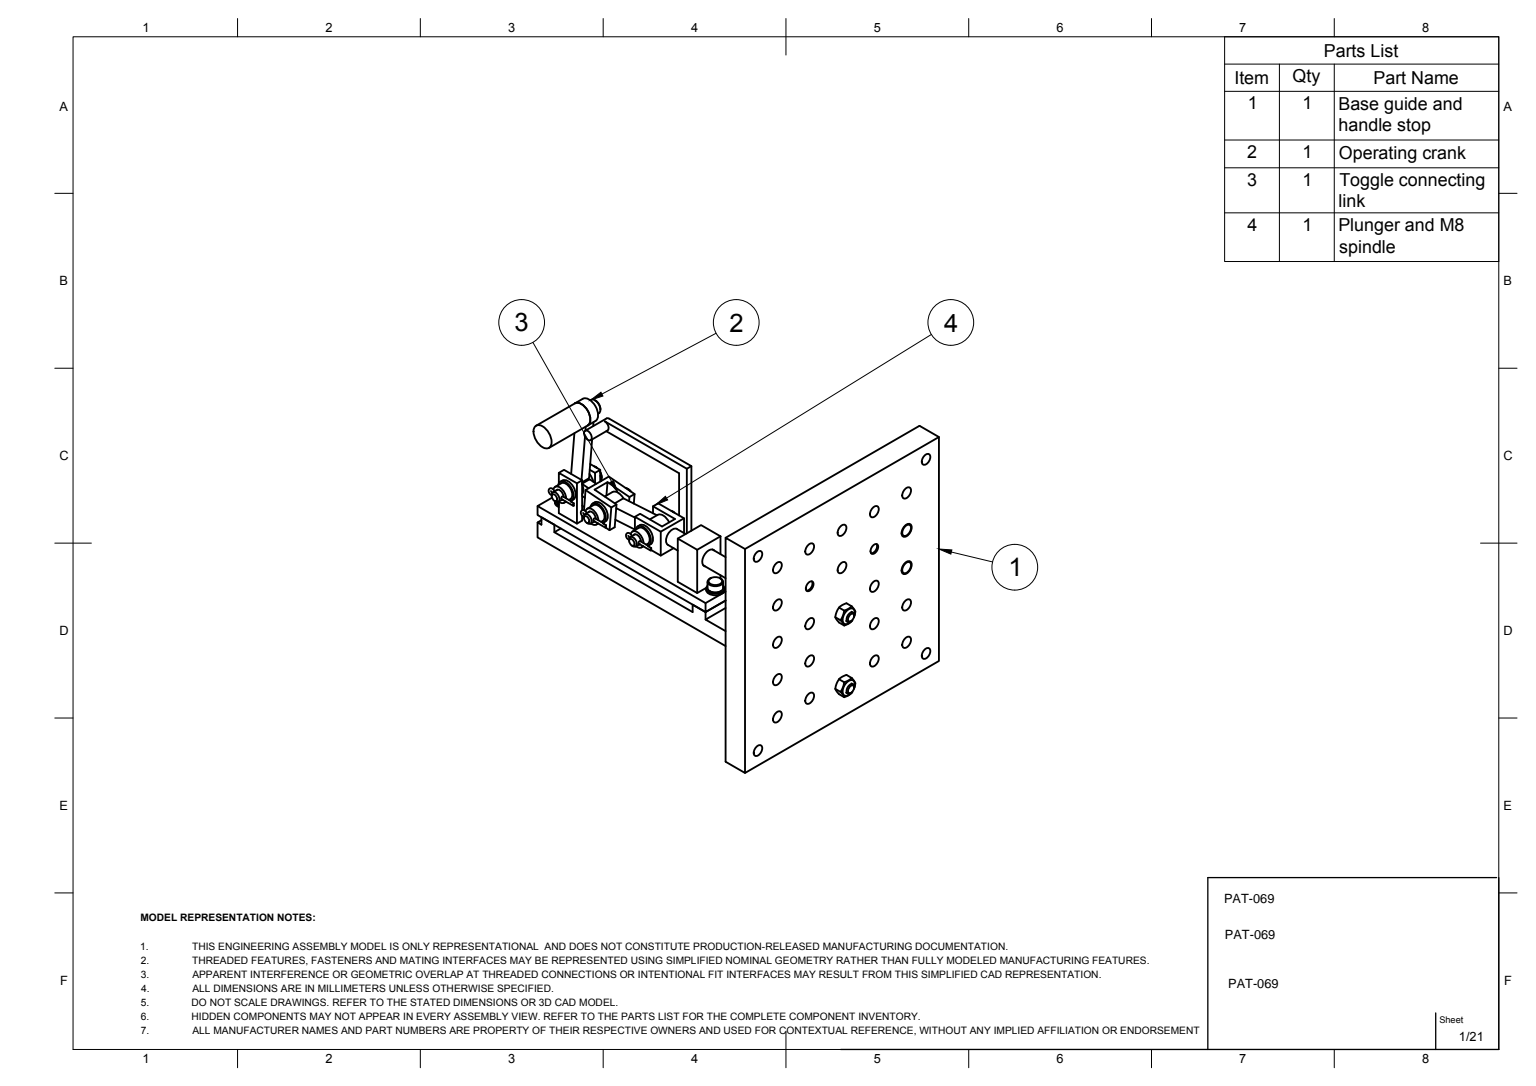
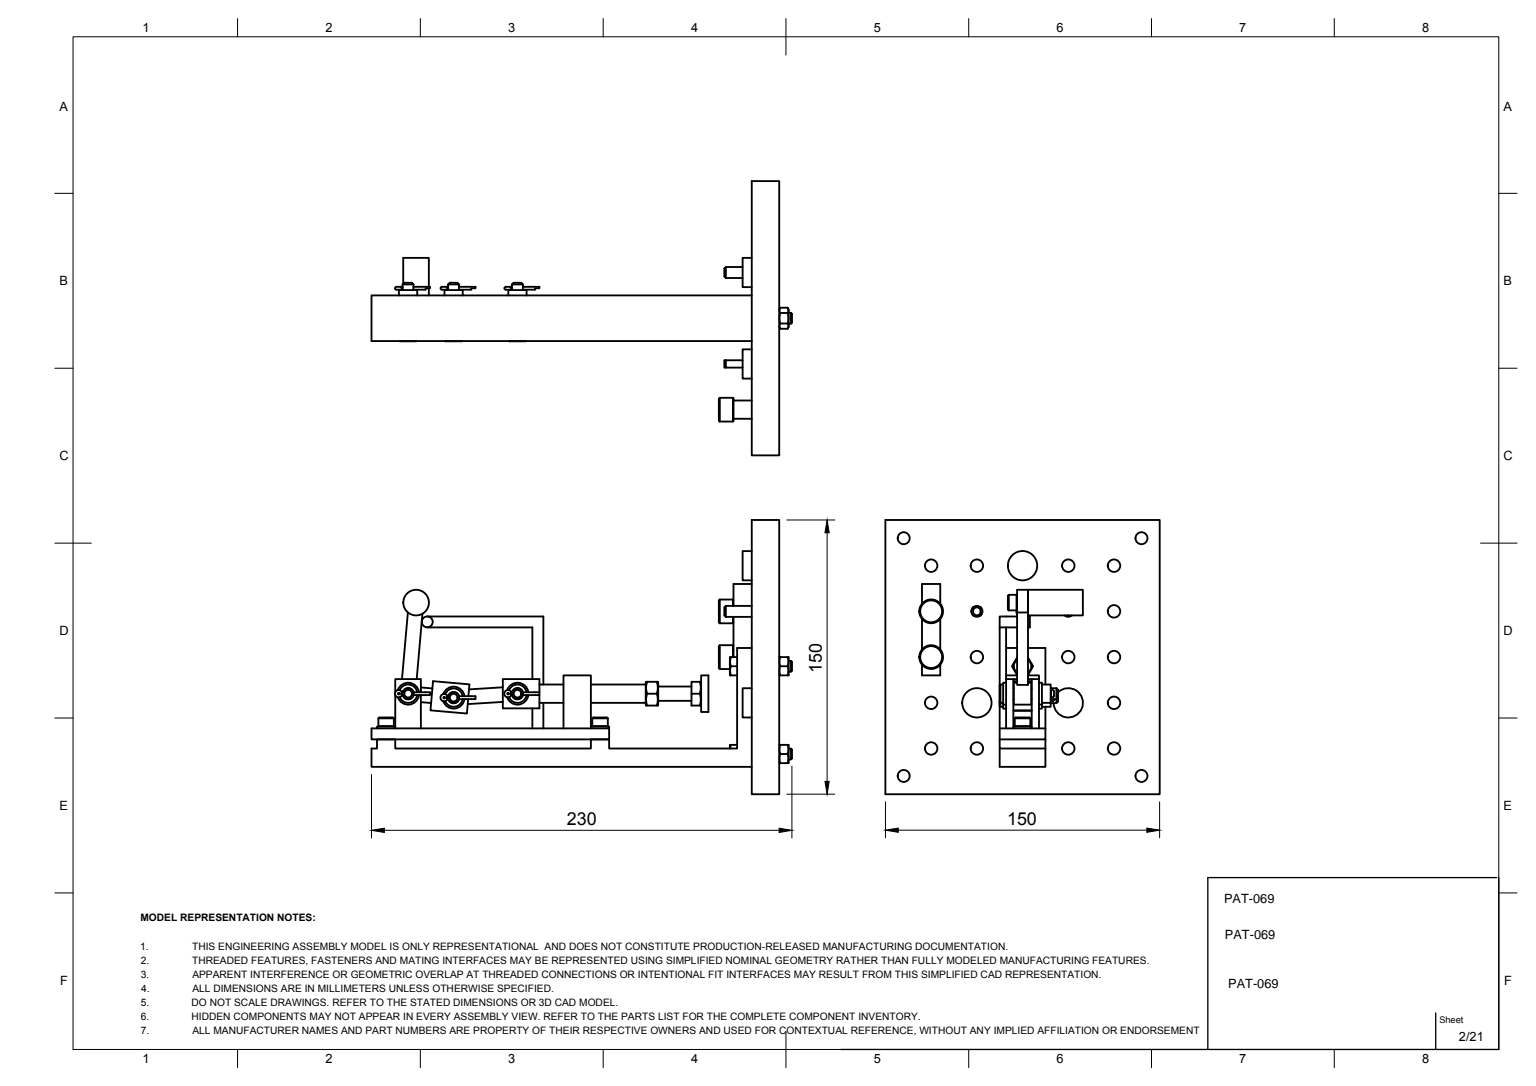
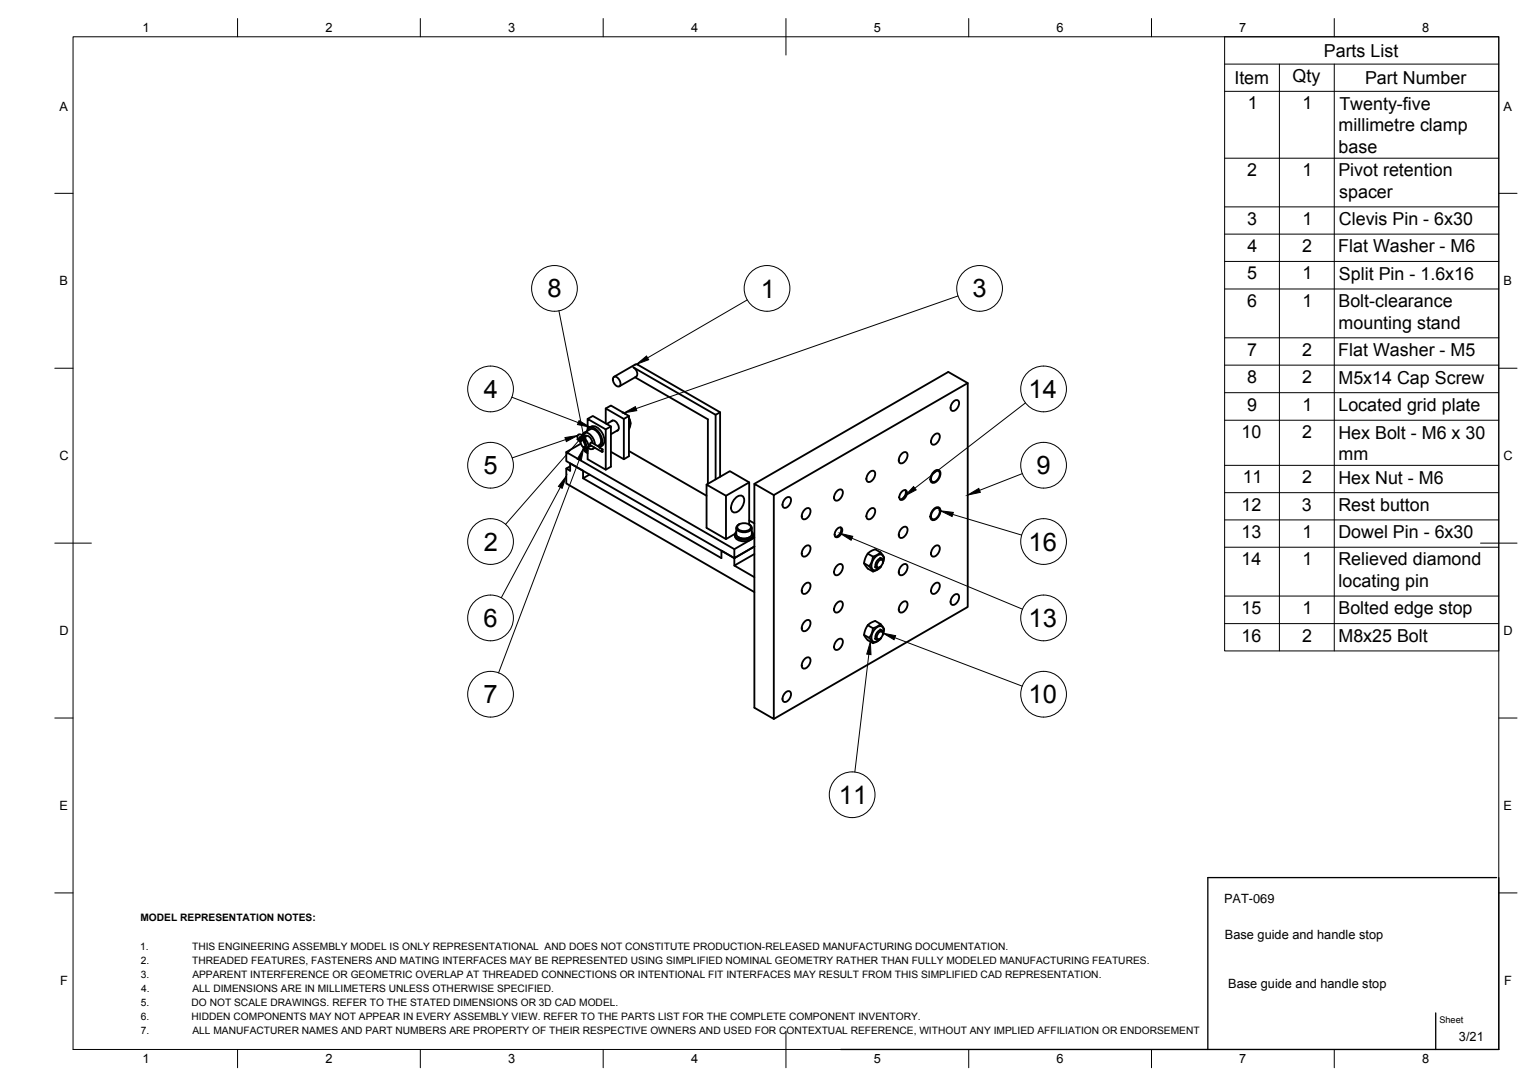
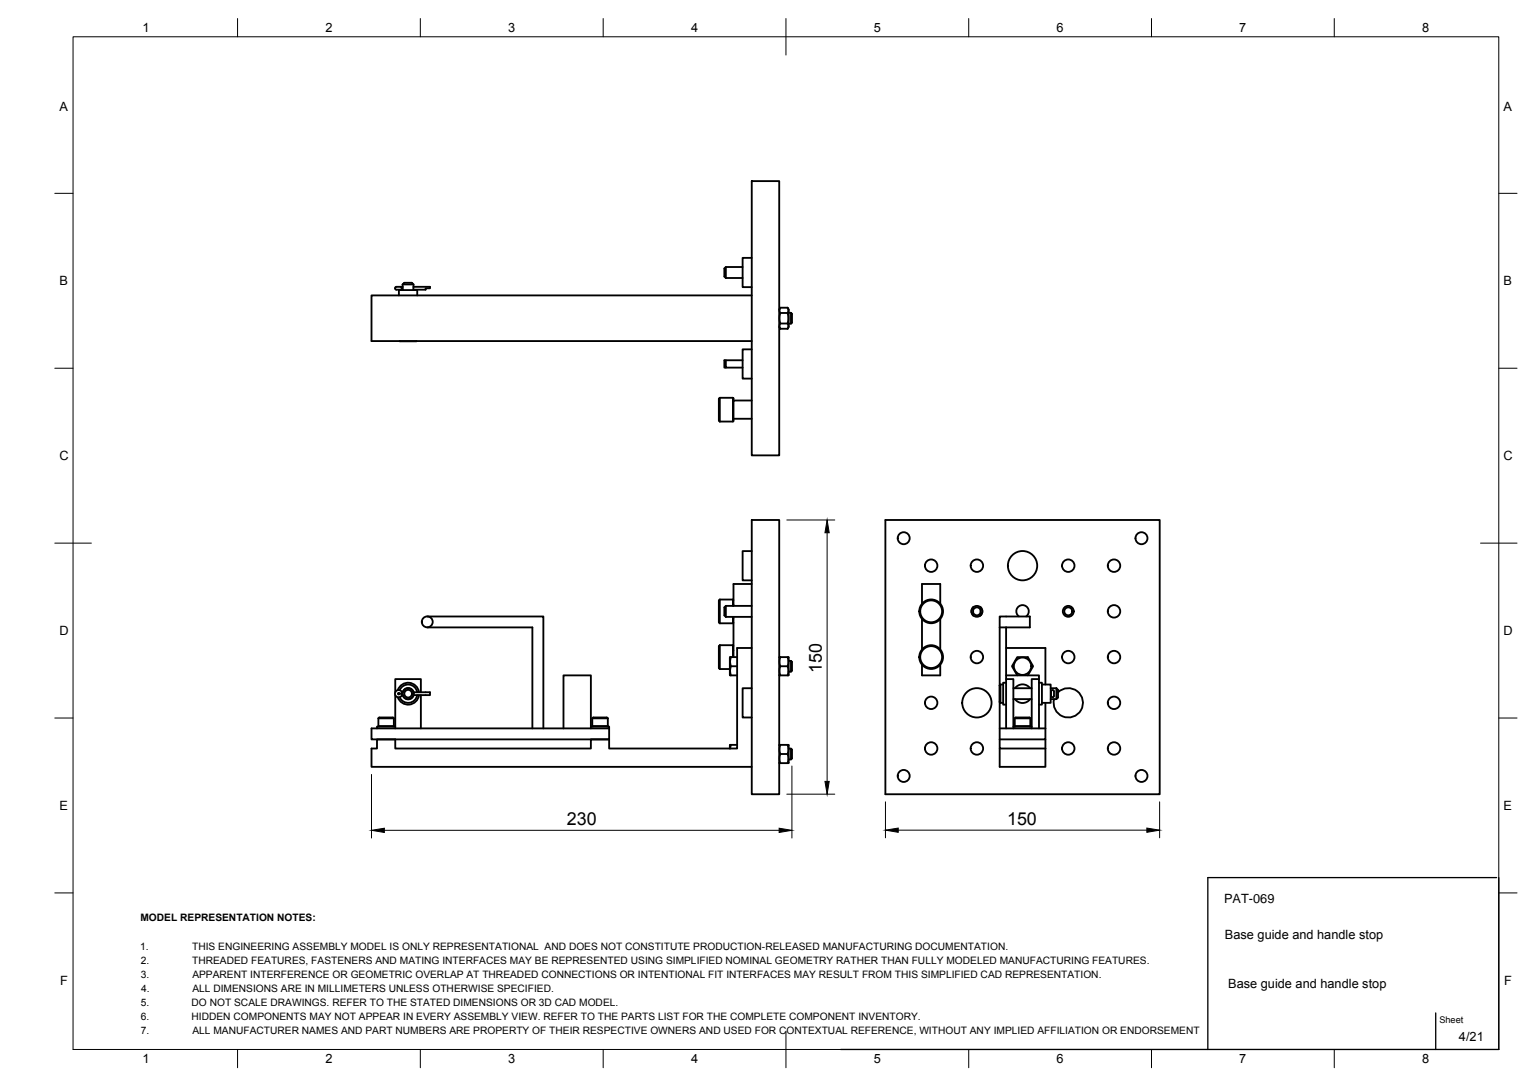
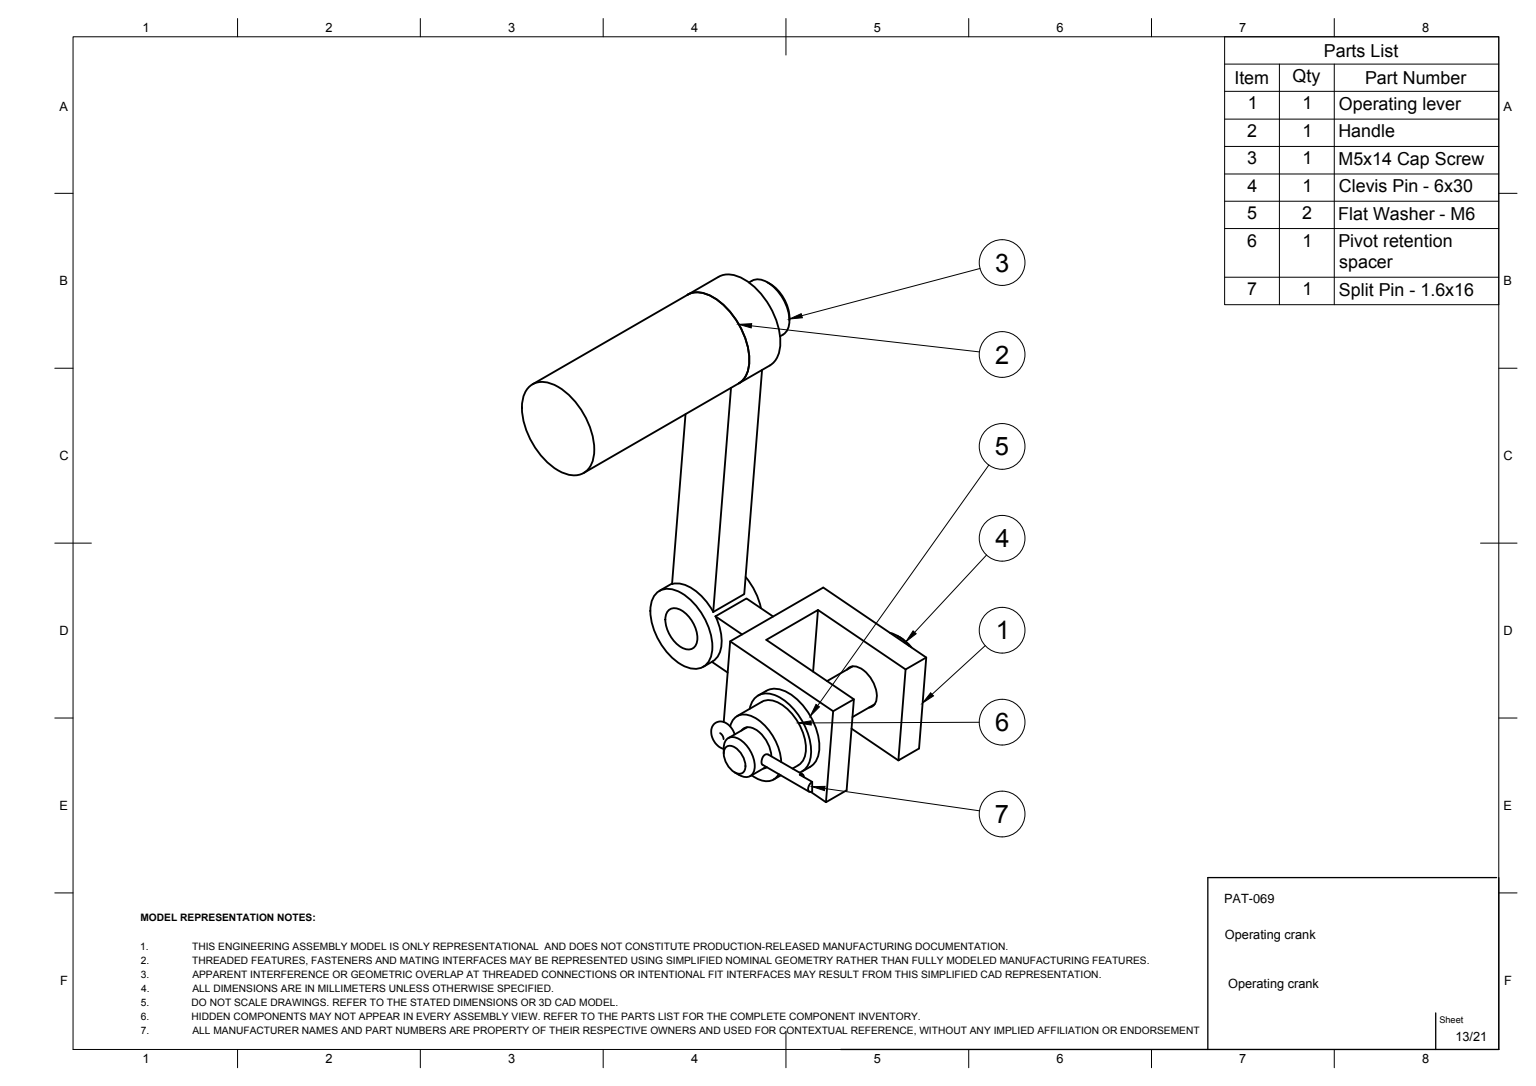
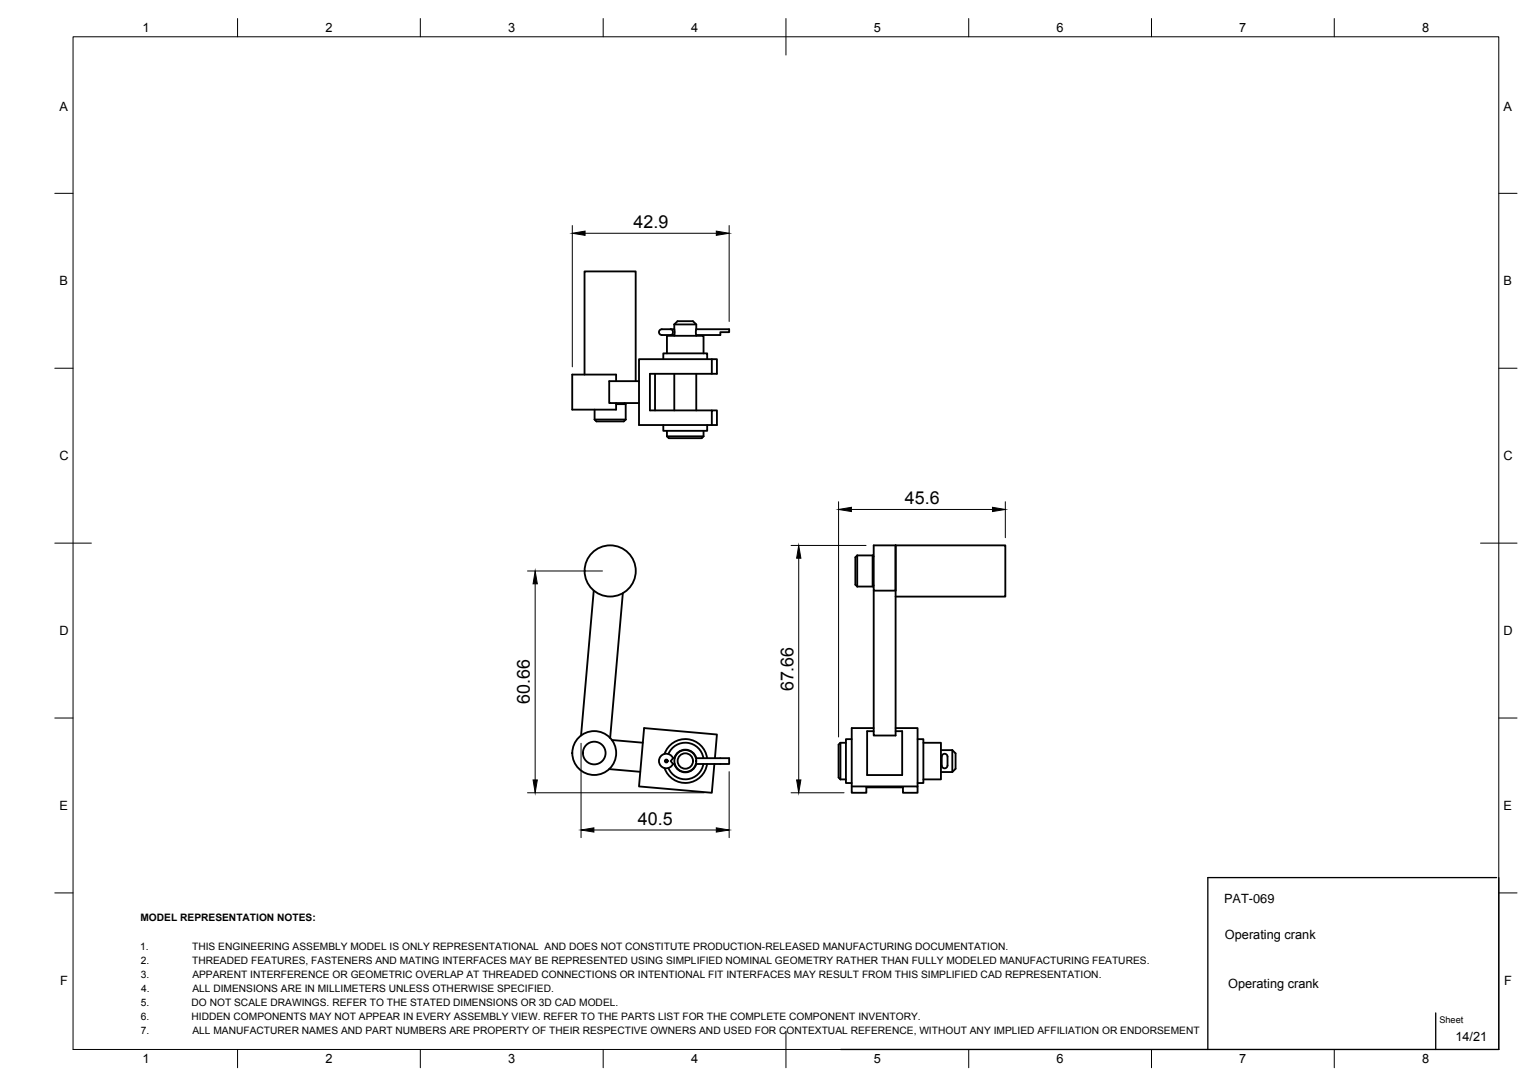
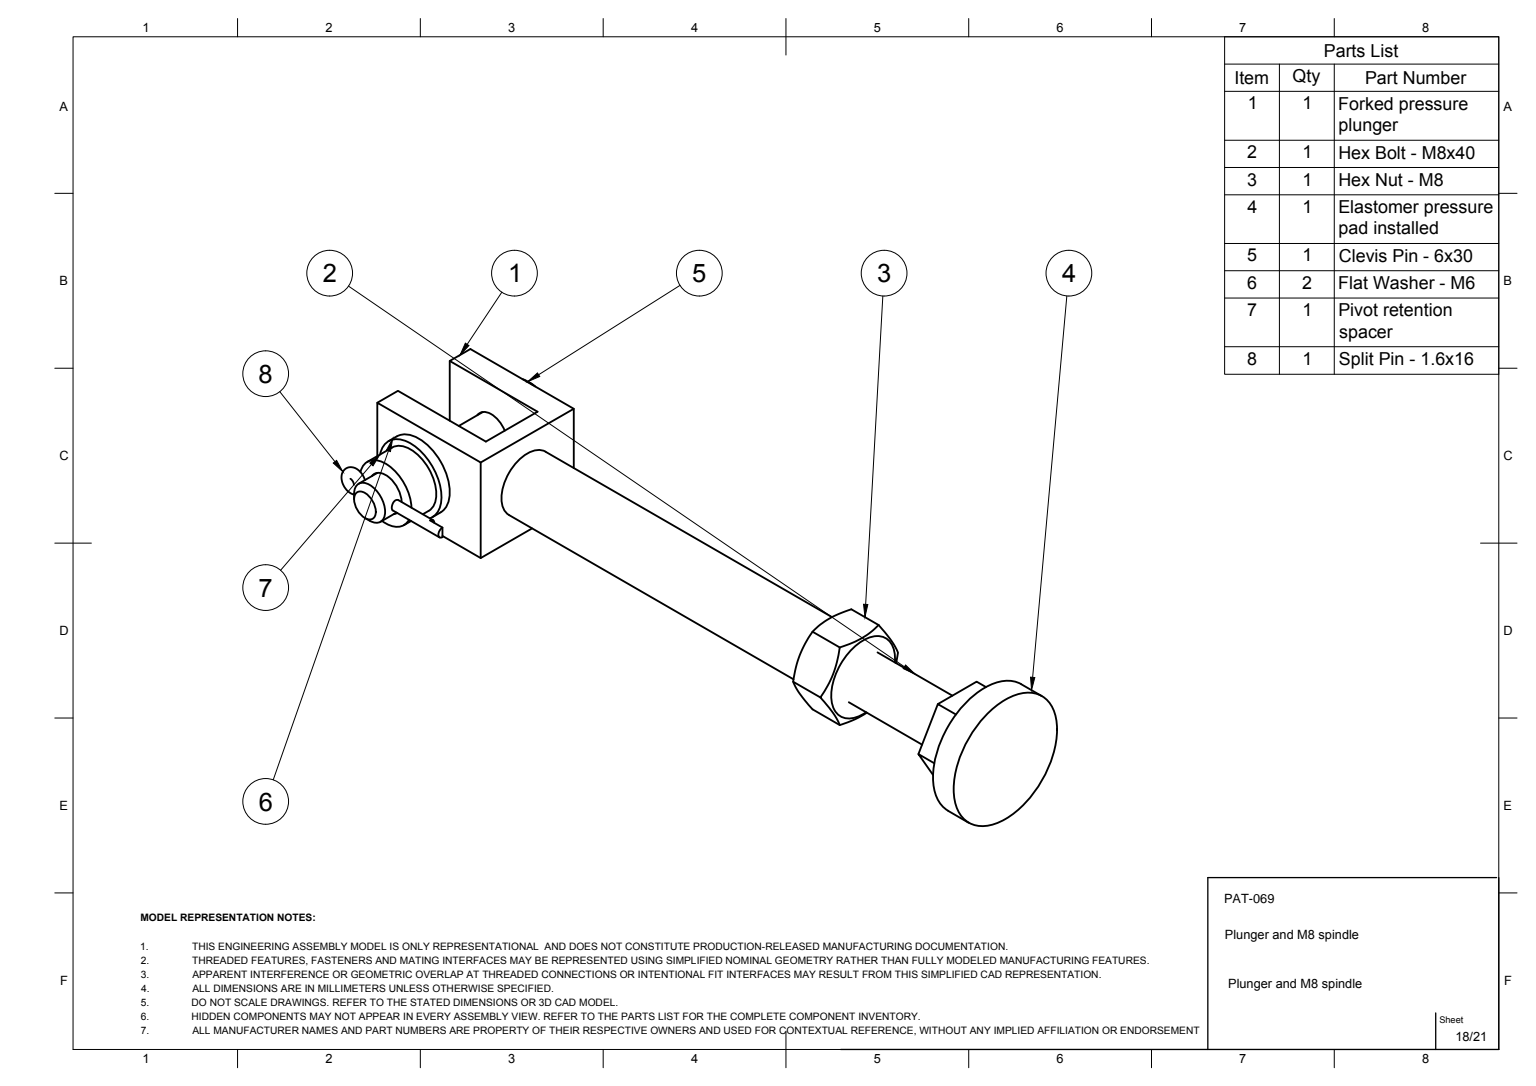
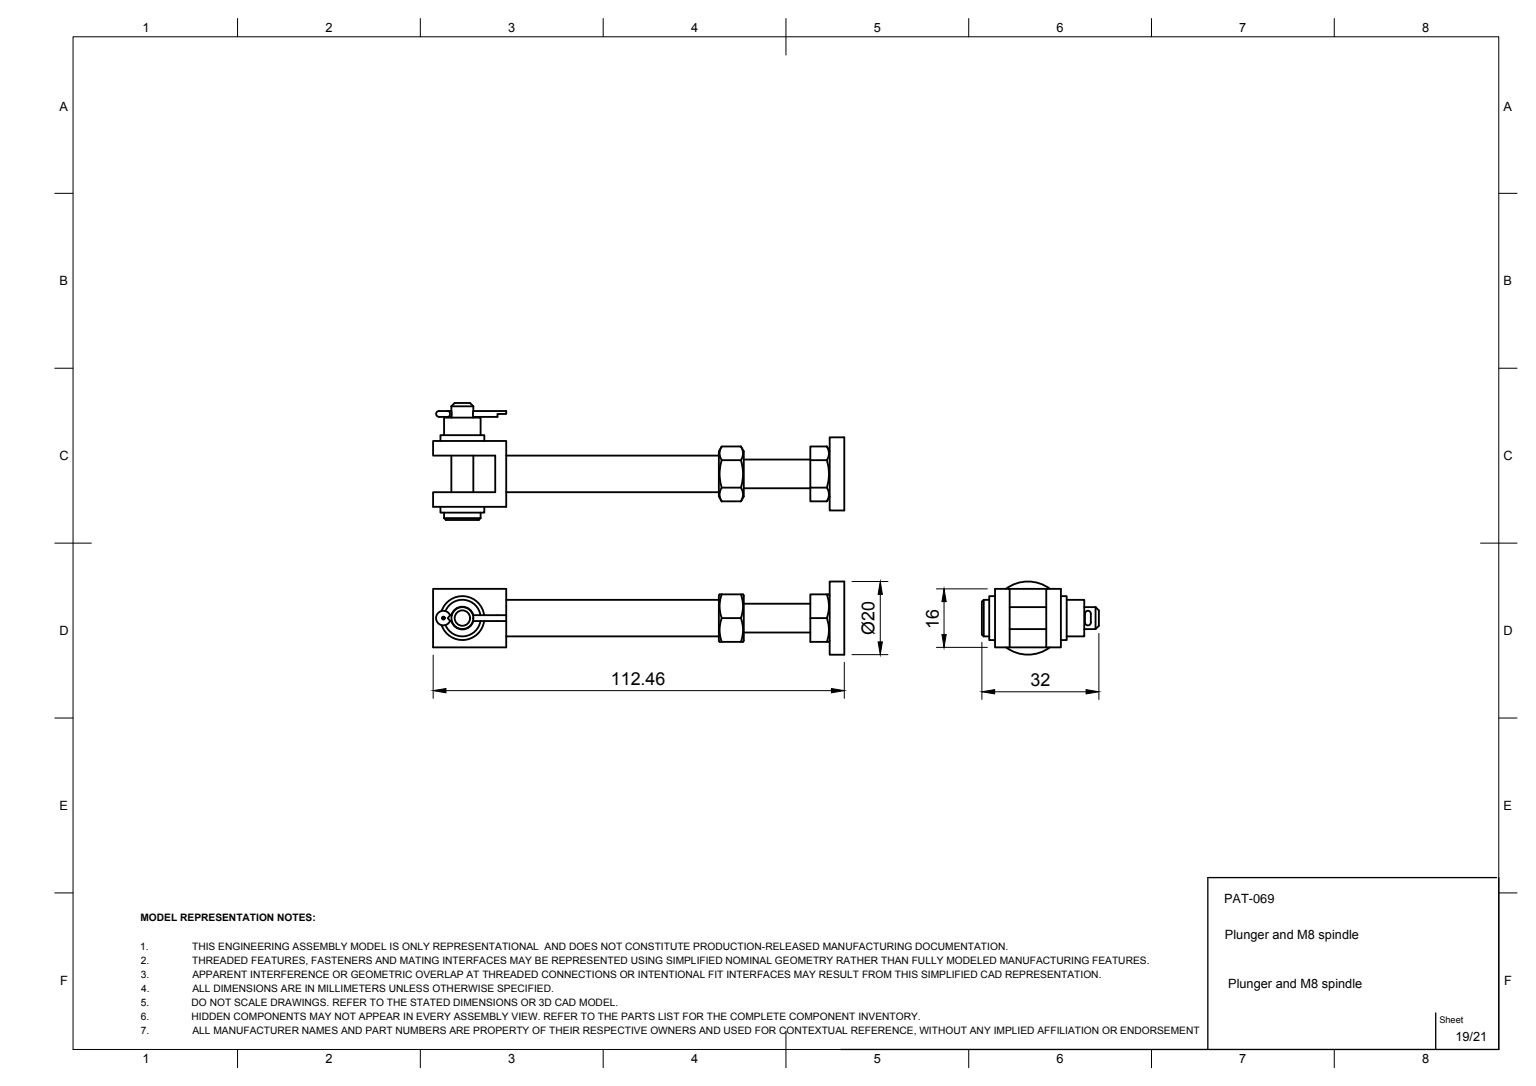
ISO-10303-21;
HEADER;
/* Generated by software containing ST-Developer
 * from STEP Tools, Inc. (www.steptools.com) 
 */

FILE_DESCRIPTION(
/* description */ ('Located fixture plate with toggle clamp'),
/* implementation_level */ '2;1');

FILE_NAME(
/* name */ 'PAT-069',
/* time_stamp */ '2026-10-27T21:36:12-07:00',
/* author */ (''),
/* organization */ (''),
/* preprocessor_version */ 'ST-DEVELOPER v20.2',
/* originating_system */ 'Autodesk Translation Framework v15.17.0.0',
/* authorisation */ '');

FILE_SCHEMA (('AUTOMOTIVE_DESIGN { 1 0 10303 214 3 1 1 }'));
ENDSEC;

DATA;
#10=MECHANICAL_DESIGN_GEOMETRIC_PRESENTATION_REPRESENTATION('',(#321,#322,
#323,#324,#325,#326,#327,#328,#329,#330,#331,#332,#333,#334,#335,#336,#337,
#338,#339,#340,#341,#342,#343,#344),#9285);
#11=TOROIDAL_SURFACE('',#5974,0.12,0.08);
#12=B_SPLINE_CURVE_WITH_KNOTS('',3,(#8976,#8977,#8978,#8979,#8980,#8981,
#8982,#8983,#8984,#8985),.UNSPECIFIED.,.F.,.F.,(4,2,2,2,4),(0.,0.0302963256060356,
0.0605926512120712,0.090883446720838,0.121174242229605),.UNSPECIFIED.);
#13=B_SPLINE_CURVE_WITH_KNOTS('',3,(#8988,#8989,#8990,#8991,#8992,#8993,
#8994,#8995,#8996,#8997,#8998,#8999,#9000,#9001,#9002,#9003,#9004,#9005,
#9006,#9007,#9008,#9009,#9010,#9011,#9012,#9013,#9014,#9015,#9016,#9017,
#9018,#9019,#9020,#9021),.UNSPECIFIED.,.T.,.F.,(4,2,2,2,2,2,2,2,2,2,2,2,
2,2,2,2,4),(0.,0.0302963256060358,0.0605926512120716,0.0908834467208383,
0.121174242229605,0.151465037738372,0.181755833247138,0.212052158853174,
0.24234848445921,0.272644810065246,0.302941135671282,0.333231931180048,
0.363522726688815,0.393813522197582,0.424104317706349,0.454400643312384,
0.48469696891842),.UNSPECIFIED.);
#14=B_SPLINE_CURVE_WITH_KNOTS('',3,(#9023,#9024,#9025,#9026,#9027,#9028,
#9029,#9030,#9031,#9032),.UNSPECIFIED.,.F.,.F.,(4,2,2,2,4),(0.363522726688815,
0.393813522197581,0.424104317706348,0.454400643312384,0.48469696891842),
 .UNSPECIFIED.);
#15=B_SPLINE_CURVE_WITH_KNOTS('',3,(#9033,#9034,#9035,#9036,#9037,#9038,
#9039,#9040,#9041,#9042,#9043,#9044,#9045,#9046,#9047,#9048,#9049,#9050),
 .UNSPECIFIED.,.F.,.F.,(4,2,2,2,2,2,2,2,4),(0.121174242229605,0.151465037738371,
0.181755833247138,0.212052158853174,0.24234848445921,0.272644810065246,
0.302941135671281,0.333231931180048,0.363522726688815),.UNSPECIFIED.);
#16=B_SPLINE_CURVE_WITH_KNOTS('',3,(#9112,#9113,#9114,#9115,#9116,#9117,
#9118,#9119,#9120,#9121,#9122,#9123,#9124,#9125,#9126,#9127,#9128,#9129,
#9130,#9131,#9132,#9133,#9134,#9135,#9136,#9137),.UNSPECIFIED.,.F.,.F.,
(4,2,2,2,2,2,2,2,2,2,2,2,4),(-0.00054581412719389,0.,0.0281583564005144,
0.0618496465371181,0.0905865724114538,0.120694112793616,0.144966158459363,
0.16923820412511,0.199345744507272,0.228082670381608,0.261773960518212,
0.289932316918681,0.290478131045882),.UNSPECIFIED.);
#17=B_SPLINE_CURVE_WITH_KNOTS('',3,(#9138,#9139,#9140,#9141,#9142,#9143,
#9144,#9145,#9146,#9147,#9148,#9149,#9150,#9151,#9152,#9153,#9154,#9155,
#9156,#9157,#9158,#9159,#9160,#9161,#9162,#9163),.UNSPECIFIED.,.F.,.F.,
(4,2,2,2,2,2,2,2,2,2,2,2,4),(-0.000545814127196571,0.,0.0281583564006391,
0.0618496465374156,0.0905865724118984,0.120694112794215,0.144966158460086,
0.169238204125958,0.199345744508275,0.228082670382758,0.261773960519534,
0.289932316920171,0.29047813104737),.UNSPECIFIED.);
#18=ITEM_DEFINED_TRANSFORMATION($,$,#5857,#5874);
#19=ITEM_DEFINED_TRANSFORMATION($,$,#5463,#5984);
#20=ITEM_DEFINED_TRANSFORMATION($,$,#5964,#5985);
#21=ITEM_DEFINED_TRANSFORMATION($,$,#5940,#5986);
#22=ITEM_DEFINED_TRANSFORMATION($,$,#5955,#5987);
#23=ITEM_DEFINED_TRANSFORMATION($,$,#5955,#5988);
#24=ITEM_DEFINED_TRANSFORMATION($,$,#5973,#5989);
#25=ITEM_DEFINED_TRANSFORMATION($,$,#5511,#5990);
#26=ITEM_DEFINED_TRANSFORMATION($,$,#5546,#5991);
#27=ITEM_DEFINED_TRANSFORMATION($,$,#5557,#5992);
#28=ITEM_DEFINED_TRANSFORMATION($,$,#5546,#5993);
#29=ITEM_DEFINED_TRANSFORMATION($,$,#5557,#5994);
#30=ITEM_DEFINED_TRANSFORMATION($,$,#5581,#5995);
#31=ITEM_DEFINED_TRANSFORMATION($,$,#5718,#5996);
#32=ITEM_DEFINED_TRANSFORMATION($,$,#5672,#5997);
#33=ITEM_DEFINED_TRANSFORMATION($,$,#5685,#5998);
#34=ITEM_DEFINED_TRANSFORMATION($,$,#5702,#5999);
#35=ITEM_DEFINED_TRANSFORMATION($,$,#5685,#6000);
#36=ITEM_DEFINED_TRANSFORMATION($,$,#5702,#6001);
#37=ITEM_DEFINED_TRANSFORMATION($,$,#5718,#6002);
#38=ITEM_DEFINED_TRANSFORMATION($,$,#5718,#6003);
#39=ITEM_DEFINED_TRANSFORMATION($,$,#5728,#6004);
#40=ITEM_DEFINED_TRANSFORMATION($,$,#5736,#6005);
#41=ITEM_DEFINED_TRANSFORMATION($,$,#5754,#6006);
#42=ITEM_DEFINED_TRANSFORMATION($,$,#5754,#6007);
#43=ITEM_DEFINED_TRANSFORMATION($,$,#5779,#6008);
#44=ITEM_DEFINED_TRANSFORMATION($,$,#5822,#6009);
#45=ITEM_DEFINED_TRANSFORMATION($,$,#5832,#6010);
#46=ITEM_DEFINED_TRANSFORMATION($,$,#5940,#6011);
#47=ITEM_DEFINED_TRANSFORMATION($,$,#5955,#6012);
#48=ITEM_DEFINED_TRANSFORMATION($,$,#5955,#6013);
#49=ITEM_DEFINED_TRANSFORMATION($,$,#5964,#6014);
#50=ITEM_DEFINED_TRANSFORMATION($,$,#5973,#6015);
#51=ITEM_DEFINED_TRANSFORMATION($,$,#5876,#6016);
#52=ITEM_DEFINED_TRANSFORMATION($,$,#5901,#6017);
#53=ITEM_DEFINED_TRANSFORMATION($,$,#5918,#6018);
#54=ITEM_DEFINED_TRANSFORMATION($,$,#5934,#6019);
#55=ITEM_DEFINED_TRANSFORMATION($,$,#5940,#6020);
#56=ITEM_DEFINED_TRANSFORMATION($,$,#5955,#6021);
#57=ITEM_DEFINED_TRANSFORMATION($,$,#5955,#6022);
#58=ITEM_DEFINED_TRANSFORMATION($,$,#5964,#6023);
#59=ITEM_DEFINED_TRANSFORMATION($,$,#5973,#6024);
#60=ITEM_DEFINED_TRANSFORMATION($,$,#5462,#6025);
#61=ITEM_DEFINED_TRANSFORMATION($,$,#5778,#6026);
#62=ITEM_DEFINED_TRANSFORMATION($,$,#5856,#6027);
#63=ITEM_DEFINED_TRANSFORMATION($,$,#5875,#6028);
#64=(
REPRESENTATION_RELATIONSHIP($,$,#9413,#9412)
REPRESENTATION_RELATIONSHIP_WITH_TRANSFORMATION(#18)
SHAPE_REPRESENTATION_RELATIONSHIP()
);
#65=(
REPRESENTATION_RELATIONSHIP($,$,#9396,#9395)
REPRESENTATION_RELATIONSHIP_WITH_TRANSFORMATION(#19)
SHAPE_REPRESENTATION_RELATIONSHIP()
);
#66=(
REPRESENTATION_RELATIONSHIP($,$,#9421,#9395)
REPRESENTATION_RELATIONSHIP_WITH_TRANSFORMATION(#20)
SHAPE_REPRESENTATION_RELATIONSHIP()
);
#67=(
REPRESENTATION_RELATIONSHIP($,$,#9419,#9395)
REPRESENTATION_RELATIONSHIP_WITH_TRANSFORMATION(#21)
SHAPE_REPRESENTATION_RELATIONSHIP()
);
#68=(
REPRESENTATION_RELATIONSHIP($,$,#9420,#9395)
REPRESENTATION_RELATIONSHIP_WITH_TRANSFORMATION(#22)
SHAPE_REPRESENTATION_RELATIONSHIP()
);
#69=(
REPRESENTATION_RELATIONSHIP($,$,#9420,#9395)
REPRESENTATION_RELATIONSHIP_WITH_TRANSFORMATION(#23)
SHAPE_REPRESENTATION_RELATIONSHIP()
);
#70=(
REPRESENTATION_RELATIONSHIP($,$,#9422,#9395)
REPRESENTATION_RELATIONSHIP_WITH_TRANSFORMATION(#24)
SHAPE_REPRESENTATION_RELATIONSHIP()
);
#71=(
REPRESENTATION_RELATIONSHIP($,$,#9397,#9395)
REPRESENTATION_RELATIONSHIP_WITH_TRANSFORMATION(#25)
SHAPE_REPRESENTATION_RELATIONSHIP()
);
#72=(
REPRESENTATION_RELATIONSHIP($,$,#9398,#9395)
REPRESENTATION_RELATIONSHIP_WITH_TRANSFORMATION(#26)
SHAPE_REPRESENTATION_RELATIONSHIP()
);
#73=(
REPRESENTATION_RELATIONSHIP($,$,#9399,#9395)
REPRESENTATION_RELATIONSHIP_WITH_TRANSFORMATION(#27)
SHAPE_REPRESENTATION_RELATIONSHIP()
);
#74=(
REPRESENTATION_RELATIONSHIP($,$,#9398,#9395)
REPRESENTATION_RELATIONSHIP_WITH_TRANSFORMATION(#28)
SHAPE_REPRESENTATION_RELATIONSHIP()
);
#75=(
REPRESENTATION_RELATIONSHIP($,$,#9399,#9395)
REPRESENTATION_RELATIONSHIP_WITH_TRANSFORMATION(#29)
SHAPE_REPRESENTATION_RELATIONSHIP()
);
#76=(
REPRESENTATION_RELATIONSHIP($,$,#9400,#9395)
REPRESENTATION_RELATIONSHIP_WITH_TRANSFORMATION(#30)
SHAPE_REPRESENTATION_RELATIONSHIP()
);
#77=(
REPRESENTATION_RELATIONSHIP($,$,#9404,#9395)
REPRESENTATION_RELATIONSHIP_WITH_TRANSFORMATION(#31)
SHAPE_REPRESENTATION_RELATIONSHIP()
);
#78=(
REPRESENTATION_RELATIONSHIP($,$,#9401,#9395)
REPRESENTATION_RELATIONSHIP_WITH_TRANSFORMATION(#32)
SHAPE_REPRESENTATION_RELATIONSHIP()
);
#79=(
REPRESENTATION_RELATIONSHIP($,$,#9402,#9395)
REPRESENTATION_RELATIONSHIP_WITH_TRANSFORMATION(#33)
SHAPE_REPRESENTATION_RELATIONSHIP()
);
#80=(
REPRESENTATION_RELATIONSHIP($,$,#9403,#9395)
REPRESENTATION_RELATIONSHIP_WITH_TRANSFORMATION(#34)
SHAPE_REPRESENTATION_RELATIONSHIP()
);
#81=(
REPRESENTATION_RELATIONSHIP($,$,#9402,#9395)
REPRESENTATION_RELATIONSHIP_WITH_TRANSFORMATION(#35)
SHAPE_REPRESENTATION_RELATIONSHIP()
);
#82=(
REPRESENTATION_RELATIONSHIP($,$,#9403,#9395)
REPRESENTATION_RELATIONSHIP_WITH_TRANSFORMATION(#36)
SHAPE_REPRESENTATION_RELATIONSHIP()
);
#83=(
REPRESENTATION_RELATIONSHIP($,$,#9404,#9395)
REPRESENTATION_RELATIONSHIP_WITH_TRANSFORMATION(#37)
SHAPE_REPRESENTATION_RELATIONSHIP()
);
#84=(
REPRESENTATION_RELATIONSHIP($,$,#9404,#9395)
REPRESENTATION_RELATIONSHIP_WITH_TRANSFORMATION(#38)
SHAPE_REPRESENTATION_RELATIONSHIP()
);
#85=(
REPRESENTATION_RELATIONSHIP($,$,#9405,#9395)
REPRESENTATION_RELATIONSHIP_WITH_TRANSFORMATION(#39)
SHAPE_REPRESENTATION_RELATIONSHIP()
);
#86=(
REPRESENTATION_RELATIONSHIP($,$,#9406,#9395)
REPRESENTATION_RELATIONSHIP_WITH_TRANSFORMATION(#40)
SHAPE_REPRESENTATION_RELATIONSHIP()
);
#87=(
REPRESENTATION_RELATIONSHIP($,$,#9407,#9395)
REPRESENTATION_RELATIONSHIP_WITH_TRANSFORMATION(#41)
SHAPE_REPRESENTATION_RELATIONSHIP()
);
#88=(
REPRESENTATION_RELATIONSHIP($,$,#9407,#9395)
REPRESENTATION_RELATIONSHIP_WITH_TRANSFORMATION(#42)
SHAPE_REPRESENTATION_RELATIONSHIP()
);
#89=(
REPRESENTATION_RELATIONSHIP($,$,#9409,#9408)
REPRESENTATION_RELATIONSHIP_WITH_TRANSFORMATION(#43)
SHAPE_REPRESENTATION_RELATIONSHIP()
);
#90=(
REPRESENTATION_RELATIONSHIP($,$,#9410,#9408)
REPRESENTATION_RELATIONSHIP_WITH_TRANSFORMATION(#44)
SHAPE_REPRESENTATION_RELATIONSHIP()
);
#91=(
REPRESENTATION_RELATIONSHIP($,$,#9411,#9408)
REPRESENTATION_RELATIONSHIP_WITH_TRANSFORMATION(#45)
SHAPE_REPRESENTATION_RELATIONSHIP()
);
#92=(
REPRESENTATION_RELATIONSHIP($,$,#9419,#9408)
REPRESENTATION_RELATIONSHIP_WITH_TRANSFORMATION(#46)
SHAPE_REPRESENTATION_RELATIONSHIP()
);
#93=(
REPRESENTATION_RELATIONSHIP($,$,#9420,#9408)
REPRESENTATION_RELATIONSHIP_WITH_TRANSFORMATION(#47)
SHAPE_REPRESENTATION_RELATIONSHIP()
);
#94=(
REPRESENTATION_RELATIONSHIP($,$,#9420,#9408)
REPRESENTATION_RELATIONSHIP_WITH_TRANSFORMATION(#48)
SHAPE_REPRESENTATION_RELATIONSHIP()
);
#95=(
REPRESENTATION_RELATIONSHIP($,$,#9421,#9408)
REPRESENTATION_RELATIONSHIP_WITH_TRANSFORMATION(#49)
SHAPE_REPRESENTATION_RELATIONSHIP()
);
#96=(
REPRESENTATION_RELATIONSHIP($,$,#9422,#9408)
REPRESENTATION_RELATIONSHIP_WITH_TRANSFORMATION(#50)
SHAPE_REPRESENTATION_RELATIONSHIP()
);
#97=(
REPRESENTATION_RELATIONSHIP($,$,#9415,#9414)
REPRESENTATION_RELATIONSHIP_WITH_TRANSFORMATION(#51)
SHAPE_REPRESENTATION_RELATIONSHIP()
);
#98=(
REPRESENTATION_RELATIONSHIP($,$,#9416,#9414)
REPRESENTATION_RELATIONSHIP_WITH_TRANSFORMATION(#52)
SHAPE_REPRESENTATION_RELATIONSHIP()
);
#99=(
REPRESENTATION_RELATIONSHIP($,$,#9417,#9414)
REPRESENTATION_RELATIONSHIP_WITH_TRANSFORMATION(#53)
SHAPE_REPRESENTATION_RELATIONSHIP()
);
#100=(
REPRESENTATION_RELATIONSHIP($,$,#9418,#9414)
REPRESENTATION_RELATIONSHIP_WITH_TRANSFORMATION(#54)
SHAPE_REPRESENTATION_RELATIONSHIP()
);
#101=(
REPRESENTATION_RELATIONSHIP($,$,#9419,#9414)
REPRESENTATION_RELATIONSHIP_WITH_TRANSFORMATION(#55)
SHAPE_REPRESENTATION_RELATIONSHIP()
);
#102=(
REPRESENTATION_RELATIONSHIP($,$,#9420,#9414)
REPRESENTATION_RELATIONSHIP_WITH_TRANSFORMATION(#56)
SHAPE_REPRESENTATION_RELATIONSHIP()
);
#103=(
REPRESENTATION_RELATIONSHIP($,$,#9420,#9414)
REPRESENTATION_RELATIONSHIP_WITH_TRANSFORMATION(#57)
SHAPE_REPRESENTATION_RELATIONSHIP()
);
#104=(
REPRESENTATION_RELATIONSHIP($,$,#9421,#9414)
REPRESENTATION_RELATIONSHIP_WITH_TRANSFORMATION(#58)
SHAPE_REPRESENTATION_RELATIONSHIP()
);
#105=(
REPRESENTATION_RELATIONSHIP($,$,#9422,#9414)
REPRESENTATION_RELATIONSHIP_WITH_TRANSFORMATION(#59)
SHAPE_REPRESENTATION_RELATIONSHIP()
);
#106=(
REPRESENTATION_RELATIONSHIP($,$,#9395,#9394)
REPRESENTATION_RELATIONSHIP_WITH_TRANSFORMATION(#60)
SHAPE_REPRESENTATION_RELATIONSHIP()
);
#107=(
REPRESENTATION_RELATIONSHIP($,$,#9408,#9394)
REPRESENTATION_RELATIONSHIP_WITH_TRANSFORMATION(#61)
SHAPE_REPRESENTATION_RELATIONSHIP()
);
#108=(
REPRESENTATION_RELATIONSHIP($,$,#9412,#9394)
REPRESENTATION_RELATIONSHIP_WITH_TRANSFORMATION(#62)
SHAPE_REPRESENTATION_RELATIONSHIP()
);
#109=(
REPRESENTATION_RELATIONSHIP($,$,#9414,#9394)
REPRESENTATION_RELATIONSHIP_WITH_TRANSFORMATION(#63)
SHAPE_REPRESENTATION_RELATIONSHIP()
);
#110=CONTEXT_DEPENDENT_SHAPE_REPRESENTATION(#64,#9339);
#111=CONTEXT_DEPENDENT_SHAPE_REPRESENTATION(#65,#9349);
#112=CONTEXT_DEPENDENT_SHAPE_REPRESENTATION(#66,#9350);
#113=CONTEXT_DEPENDENT_SHAPE_REPRESENTATION(#67,#9351);
#114=CONTEXT_DEPENDENT_SHAPE_REPRESENTATION(#68,#9352);
#115=CONTEXT_DEPENDENT_SHAPE_REPRESENTATION(#69,#9353);
#116=CONTEXT_DEPENDENT_SHAPE_REPRESENTATION(#70,#9354);
#117=CONTEXT_DEPENDENT_SHAPE_REPRESENTATION(#71,#9355);
#118=CONTEXT_DEPENDENT_SHAPE_REPRESENTATION(#72,#9356);
#119=CONTEXT_DEPENDENT_SHAPE_REPRESENTATION(#73,#9357);
#120=CONTEXT_DEPENDENT_SHAPE_REPRESENTATION(#74,#9358);
#121=CONTEXT_DEPENDENT_SHAPE_REPRESENTATION(#75,#9359);
#122=CONTEXT_DEPENDENT_SHAPE_REPRESENTATION(#76,#9360);
#123=CONTEXT_DEPENDENT_SHAPE_REPRESENTATION(#77,#9361);
#124=CONTEXT_DEPENDENT_SHAPE_REPRESENTATION(#78,#9362);
#125=CONTEXT_DEPENDENT_SHAPE_REPRESENTATION(#79,#9363);
#126=CONTEXT_DEPENDENT_SHAPE_REPRESENTATION(#80,#9364);
#127=CONTEXT_DEPENDENT_SHAPE_REPRESENTATION(#81,#9365);
#128=CONTEXT_DEPENDENT_SHAPE_REPRESENTATION(#82,#9366);
#129=CONTEXT_DEPENDENT_SHAPE_REPRESENTATION(#83,#9367);
#130=CONTEXT_DEPENDENT_SHAPE_REPRESENTATION(#84,#9368);
#131=CONTEXT_DEPENDENT_SHAPE_REPRESENTATION(#85,#9369);
#132=CONTEXT_DEPENDENT_SHAPE_REPRESENTATION(#86,#9370);
#133=CONTEXT_DEPENDENT_SHAPE_REPRESENTATION(#87,#9371);
#134=CONTEXT_DEPENDENT_SHAPE_REPRESENTATION(#88,#9372);
#135=CONTEXT_DEPENDENT_SHAPE_REPRESENTATION(#89,#9373);
#136=CONTEXT_DEPENDENT_SHAPE_REPRESENTATION(#90,#9374);
#137=CONTEXT_DEPENDENT_SHAPE_REPRESENTATION(#91,#9375);
#138=CONTEXT_DEPENDENT_SHAPE_REPRESENTATION(#92,#9376);
#139=CONTEXT_DEPENDENT_SHAPE_REPRESENTATION(#93,#9377);
#140=CONTEXT_DEPENDENT_SHAPE_REPRESENTATION(#94,#9378);
#141=CONTEXT_DEPENDENT_SHAPE_REPRESENTATION(#95,#9379);
#142=CONTEXT_DEPENDENT_SHAPE_REPRESENTATION(#96,#9380);
#143=CONTEXT_DEPENDENT_SHAPE_REPRESENTATION(#97,#9381);
#144=CONTEXT_DEPENDENT_SHAPE_REPRESENTATION(#98,#9382);
#145=CONTEXT_DEPENDENT_SHAPE_REPRESENTATION(#99,#9383);
#146=CONTEXT_DEPENDENT_SHAPE_REPRESENTATION(#100,#9384);
#147=CONTEXT_DEPENDENT_SHAPE_REPRESENTATION(#101,#9385);
#148=CONTEXT_DEPENDENT_SHAPE_REPRESENTATION(#102,#9386);
#149=CONTEXT_DEPENDENT_SHAPE_REPRESENTATION(#103,#9387);
#150=CONTEXT_DEPENDENT_SHAPE_REPRESENTATION(#104,#9388);
#151=CONTEXT_DEPENDENT_SHAPE_REPRESENTATION(#105,#9389);
#152=CONTEXT_DEPENDENT_SHAPE_REPRESENTATION(#106,#9390);
#153=CONTEXT_DEPENDENT_SHAPE_REPRESENTATION(#107,#9391);
#154=CONTEXT_DEPENDENT_SHAPE_REPRESENTATION(#108,#9392);
#155=CONTEXT_DEPENDENT_SHAPE_REPRESENTATION(#109,#9393);
#156=NEXT_ASSEMBLY_USAGE_OCCURRENCE(
'Thirty-five millimetre toggle link:1',
'Thirty-five millimetre toggle link:1',
'Thirty-five millimetre toggle link:1',#9442,#9443,
'Thirty-five millimetre toggle link:1');
#157=NEXT_ASSEMBLY_USAGE_OCCURRENCE(
'Twenty-five millimetre clamp base:1',
'Twenty-five millimetre clamp base:1',
'Twenty-five millimetre clamp base:1',#9425,#9426,
'Twenty-five millimetre clamp base:1');
#158=NEXT_ASSEMBLY_USAGE_OCCURRENCE('Pivot retention spacer:1',
'Pivot retention spacer:1','Pivot retention spacer:1',#9425,#9451,
'Pivot retention spacer:1');
#159=NEXT_ASSEMBLY_USAGE_OCCURRENCE('Clevis Pin - 6x30:2',
'Clevis Pin - 6x30:2','Clevis Pin - 6x30:2',#9425,#9449,
'Clevis Pin - 6x30:2');
#160=NEXT_ASSEMBLY_USAGE_OCCURRENCE('Flat Washer - M6:2',
'Flat Washer - M6:2','Flat Washer - M6:2',#9425,#9450,
'Flat Washer - M6:2');
#161=NEXT_ASSEMBLY_USAGE_OCCURRENCE('Flat Washer - M6:3',
'Flat Washer - M6:3','Flat Washer - M6:3',#9425,#9450,
'Flat Washer - M6:3');
#162=NEXT_ASSEMBLY_USAGE_OCCURRENCE('Split Pin - 1.6x16:2',
'Split Pin - 1.6x16:2','Split Pin - 1.6x16:2',#9425,#9452,
'Split Pin - 1.6x16:2');
#163=NEXT_ASSEMBLY_USAGE_OCCURRENCE('Bolt-clearance mounting stand:1',
'Bolt-clearance mounting stand:1','Bolt-clearance mounting stand:1',#9425,
#9427,'Bolt-clearance mounting stand:1');
#164=NEXT_ASSEMBLY_USAGE_OCCURRENCE('Flat Washer - M5:2',
'Flat Washer - M5:2','Flat Washer - M5:2',#9425,#9428,
'Flat Washer - M5:2');
#165=NEXT_ASSEMBLY_USAGE_OCCURRENCE('M5x14 Cap Screw:2',
'M5x14 Cap Screw:2','M5x14 Cap Screw:2',#9425,#9429,'M5x14 Cap Screw:2');
#166=NEXT_ASSEMBLY_USAGE_OCCURRENCE('Flat Washer - M5:3',
'Flat Washer - M5:3','Flat Washer - M5:3',#9425,#9428,
'Flat Washer - M5:3');
#167=NEXT_ASSEMBLY_USAGE_OCCURRENCE('M5x14 Cap Screw:3',
'M5x14 Cap Screw:3','M5x14 Cap Screw:3',#9425,#9429,'M5x14 Cap Screw:3');
#168=NEXT_ASSEMBLY_USAGE_OCCURRENCE('Located grid plate:1',
'Located grid plate:1','Located grid plate:1',#9425,#9430,
'Located grid plate:1');
#169=NEXT_ASSEMBLY_USAGE_OCCURRENCE('Rest button:1','Rest button:1',
'Rest button:1',#9425,#9434,'Rest button:1');
#170=NEXT_ASSEMBLY_USAGE_OCCURRENCE('Bolted edge stop:1',
'Bolted edge stop:1','Bolted edge stop:1',#9425,#9431,
'Bolted edge stop:1');
#171=NEXT_ASSEMBLY_USAGE_OCCURRENCE('Hex Bolt - M6 x 30 mm:2',
'Hex Bolt - M6 x 30 mm:2','Hex Bolt - M6 x 30 mm:2',#9425,#9432,
'Hex Bolt - M6 x 30 mm:2');
#172=NEXT_ASSEMBLY_USAGE_OCCURRENCE('Hex Nut - M6:2','Hex Nut - M6:2',
'Hex Nut - M6:2',#9425,#9433,'Hex Nut - M6:2');
#173=NEXT_ASSEMBLY_USAGE_OCCURRENCE('Hex Bolt - M6 x 30 mm:3',
'Hex Bolt - M6 x 30 mm:3','Hex Bolt - M6 x 30 mm:3',#9425,#9432,
'Hex Bolt - M6 x 30 mm:3');
#174=NEXT_ASSEMBLY_USAGE_OCCURRENCE('Hex Nut - M6:3','Hex Nut - M6:3',
'Hex Nut - M6:3',#9425,#9433,'Hex Nut - M6:3');
#175=NEXT_ASSEMBLY_USAGE_OCCURRENCE('Rest button:2','Rest button:2',
'Rest button:2',#9425,#9434,'Rest button:2');
#176=NEXT_ASSEMBLY_USAGE_OCCURRENCE('Rest button:3','Rest button:3',
'Rest button:3',#9425,#9434,'Rest button:3');
#177=NEXT_ASSEMBLY_USAGE_OCCURRENCE('Dowel Pin - 6x30:2',
'Dowel Pin - 6x30:2','Dowel Pin - 6x30:2',#9425,#9435,
'Dowel Pin - 6x30:2');
#178=NEXT_ASSEMBLY_USAGE_OCCURRENCE('Relieved diamond locating pin:2',
'Relieved diamond locating pin:2','Relieved diamond locating pin:2',#9425,
#9436,'Relieved diamond locating pin:2');
#179=NEXT_ASSEMBLY_USAGE_OCCURRENCE('M8x25 Bolt:2','M8x25 Bolt:2',
'M8x25 Bolt:2',#9425,#9437,'M8x25 Bolt:2');
#180=NEXT_ASSEMBLY_USAGE_OCCURRENCE('M8x25 Bolt:3','M8x25 Bolt:3',
'M8x25 Bolt:3',#9425,#9437,'M8x25 Bolt:3');
#181=NEXT_ASSEMBLY_USAGE_OCCURRENCE('Operating lever:1',
'Operating lever:1','Operating lever:1',#9438,#9439,'Operating lever:1');
#182=NEXT_ASSEMBLY_USAGE_OCCURRENCE('Handle:2','Handle:2','Handle:2',#9438,
#9440,'Handle:2');
#183=NEXT_ASSEMBLY_USAGE_OCCURRENCE('M5x14 Cap Screw (1):2',
'M5x14 Cap Screw (1):2','M5x14 Cap Screw (1):2',#9438,#9441,
'M5x14 Cap Screw (1):2');
#184=NEXT_ASSEMBLY_USAGE_OCCURRENCE('Clevis Pin - 6x30:3',
'Clevis Pin - 6x30:3','Clevis Pin - 6x30:3',#9438,#9449,
'Clevis Pin - 6x30:3');
#185=NEXT_ASSEMBLY_USAGE_OCCURRENCE('Flat Washer - M6:4',
'Flat Washer - M6:4','Flat Washer - M6:4',#9438,#9450,
'Flat Washer - M6:4');
#186=NEXT_ASSEMBLY_USAGE_OCCURRENCE('Flat Washer - M6:5',
'Flat Washer - M6:5','Flat Washer - M6:5',#9438,#9450,
'Flat Washer - M6:5');
#187=NEXT_ASSEMBLY_USAGE_OCCURRENCE('Pivot retention spacer:2',
'Pivot retention spacer:2','Pivot retention spacer:2',#9438,#9451,
'Pivot retention spacer:2');
#188=NEXT_ASSEMBLY_USAGE_OCCURRENCE('Split Pin - 1.6x16:3',
'Split Pin - 1.6x16:3','Split Pin - 1.6x16:3',#9438,#9452,
'Split Pin - 1.6x16:3');
#189=NEXT_ASSEMBLY_USAGE_OCCURRENCE('Forked pressure plunger:1',
'Forked pressure plunger:1','Forked pressure plunger:1',#9444,#9445,
'Forked pressure plunger:1');
#190=NEXT_ASSEMBLY_USAGE_OCCURRENCE('Hex Bolt - M8x40:2',
'Hex Bolt - M8x40:2','Hex Bolt - M8x40:2',#9444,#9446,
'Hex Bolt - M8x40:2');
#191=NEXT_ASSEMBLY_USAGE_OCCURRENCE('Hex Nut - M8:2','Hex Nut - M8:2',
'Hex Nut - M8:2',#9444,#9447,'Hex Nut - M8:2');
#192=NEXT_ASSEMBLY_USAGE_OCCURRENCE(
'Elastomer pressure pad installed:2',
'Elastomer pressure pad installed:2',
'Elastomer pressure pad installed:2',#9444,#9448,
'Elastomer pressure pad installed:2');
#193=NEXT_ASSEMBLY_USAGE_OCCURRENCE('Clevis Pin - 6x30:4',
'Clevis Pin - 6x30:4','Clevis Pin - 6x30:4',#9444,#9449,
'Clevis Pin - 6x30:4');
#194=NEXT_ASSEMBLY_USAGE_OCCURRENCE('Flat Washer - M6:6',
'Flat Washer - M6:6','Flat Washer - M6:6',#9444,#9450,
'Flat Washer - M6:6');
#195=NEXT_ASSEMBLY_USAGE_OCCURRENCE('Flat Washer - M6:7',
'Flat Washer - M6:7','Flat Washer - M6:7',#9444,#9450,
'Flat Washer - M6:7');
#196=NEXT_ASSEMBLY_USAGE_OCCURRENCE('Pivot retention spacer:3',
'Pivot retention spacer:3','Pivot retention spacer:3',#9444,#9451,
'Pivot retention spacer:3');
#197=NEXT_ASSEMBLY_USAGE_OCCURRENCE('Split Pin - 1.6x16:4',
'Split Pin - 1.6x16:4','Split Pin - 1.6x16:4',#9444,#9452,
'Split Pin - 1.6x16:4');
#198=NEXT_ASSEMBLY_USAGE_OCCURRENCE('Base guide and handle stop:1',
'Base guide and handle stop:1','Base guide and handle stop:1',#9424,#9425,
'Base guide and handle stop:1');
#199=NEXT_ASSEMBLY_USAGE_OCCURRENCE('Operating crank:1',
'Operating crank:1','Operating crank:1',#9424,#9438,'Operating crank:1');
#200=NEXT_ASSEMBLY_USAGE_OCCURRENCE('Toggle connecting link:1',
'Toggle connecting link:1','Toggle connecting link:1',#9424,#9442,
'Toggle connecting link:1');
#201=NEXT_ASSEMBLY_USAGE_OCCURRENCE('Plunger and M8 spindle:1',
'Plunger and M8 spindle:1','Plunger and M8 spindle:1',#9424,#9444,
'Plunger and M8 spindle:1');
#202=SPHERICAL_SURFACE('',#5729,0.600000000000005);
#203=SPHERICAL_SURFACE('',#5752,0.600000000000005);
#204=(
BOUNDED_CURVE()
B_SPLINE_CURVE(2,(#8213,#8214,#8215),.UNSPECIFIED.,.F.,.F.)
B_SPLINE_CURVE_WITH_KNOTS((3,3),(0.144988513094728,0.791574906712449),
 .UNSPECIFIED.)
CURVE()
GEOMETRIC_REPRESENTATION_ITEM()
RATIONAL_B_SPLINE_CURVE((1.09282032302755,1.26188021535082,1.09282032302931))
REPRESENTATION_ITEM('')
);
#205=(
BOUNDED_CURVE()
B_SPLINE_CURVE(2,(#8217,#8218,#8219),.UNSPECIFIED.,.F.,.F.)
B_SPLINE_CURVE_WITH_KNOTS((3,3),(0.144988513094728,0.791574906712449),
 .UNSPECIFIED.)
CURVE()
GEOMETRIC_REPRESENTATION_ITEM()
RATIONAL_B_SPLINE_CURVE((1.09282032302755,1.26188021535082,1.09282032302931))
REPRESENTATION_ITEM('')
);
#206=(
BOUNDED_CURVE()
B_SPLINE_CURVE(2,(#8221,#8222,#8223),.UNSPECIFIED.,.F.,.F.)
B_SPLINE_CURVE_WITH_KNOTS((3,3),(0.144988513094728,0.791574906712449),
 .UNSPECIFIED.)
CURVE()
GEOMETRIC_REPRESENTATION_ITEM()
RATIONAL_B_SPLINE_CURVE((1.09282032302755,1.26188021535082,1.09282032302931))
REPRESENTATION_ITEM('')
);
#207=(
BOUNDED_CURVE()
B_SPLINE_CURVE(2,(#8225,#8226,#8227),.UNSPECIFIED.,.F.,.F.)
B_SPLINE_CURVE_WITH_KNOTS((3,3),(0.144988513094728,0.791574906712449),
 .UNSPECIFIED.)
CURVE()
GEOMETRIC_REPRESENTATION_ITEM()
RATIONAL_B_SPLINE_CURVE((1.09282032302755,1.26188021535082,1.09282032302931))
REPRESENTATION_ITEM('')
);
#208=(
BOUNDED_CURVE()
B_SPLINE_CURVE(2,(#8229,#8230,#8231),.UNSPECIFIED.,.F.,.F.)
B_SPLINE_CURVE_WITH_KNOTS((3,3),(0.144988513094728,0.791574906712449),
 .UNSPECIFIED.)
CURVE()
GEOMETRIC_REPRESENTATION_ITEM()
RATIONAL_B_SPLINE_CURVE((1.09282032302755,1.26188021535082,1.09282032302931))
REPRESENTATION_ITEM('')
);
#209=(
BOUNDED_CURVE()
B_SPLINE_CURVE(2,(#8232,#8233,#8234),.UNSPECIFIED.,.F.,.F.)
B_SPLINE_CURVE_WITH_KNOTS((3,3),(0.144988513094727,0.791574906712449),
 .UNSPECIFIED.)
CURVE()
GEOMETRIC_REPRESENTATION_ITEM()
RATIONAL_B_SPLINE_CURVE((1.09282032302755,1.26188021535082,1.09282032302931))
REPRESENTATION_ITEM('')
);
#210=(
BOUNDED_CURVE()
B_SPLINE_CURVE(2,(#8265,#8266,#8267),.UNSPECIFIED.,.F.,.F.)
B_SPLINE_CURVE_WITH_KNOTS((3,3),(0.144988513094728,0.791574906712449),
 .UNSPECIFIED.)
CURVE()
GEOMETRIC_REPRESENTATION_ITEM()
RATIONAL_B_SPLINE_CURVE((1.09282032302755,1.26188021535082,1.09282032302931))
REPRESENTATION_ITEM('')
);
#211=(
BOUNDED_CURVE()
B_SPLINE_CURVE(2,(#8269,#8270,#8271),.UNSPECIFIED.,.F.,.F.)
B_SPLINE_CURVE_WITH_KNOTS((3,3),(0.144988513094728,0.791574906712449),
 .UNSPECIFIED.)
CURVE()
GEOMETRIC_REPRESENTATION_ITEM()
RATIONAL_B_SPLINE_CURVE((1.09282032302755,1.26188021535082,1.09282032302931))
REPRESENTATION_ITEM('')
);
#212=(
BOUNDED_CURVE()
B_SPLINE_CURVE(2,(#8276,#8277,#8278),.UNSPECIFIED.,.F.,.F.)
B_SPLINE_CURVE_WITH_KNOTS((3,3),(0.144988513094728,0.791574906712449),
 .UNSPECIFIED.)
CURVE()
GEOMETRIC_REPRESENTATION_ITEM()
RATIONAL_B_SPLINE_CURVE((1.09282032302755,1.26188021535082,1.09282032302931))
REPRESENTATION_ITEM('')
);
#213=(
BOUNDED_CURVE()
B_SPLINE_CURVE(2,(#8280,#8281,#8282),.UNSPECIFIED.,.F.,.F.)
B_SPLINE_CURVE_WITH_KNOTS((3,3),(0.144988513094728,0.791574906712449),
 .UNSPECIFIED.)
CURVE()
GEOMETRIC_REPRESENTATION_ITEM()
RATIONAL_B_SPLINE_CURVE((1.09282032302755,1.26188021535082,1.09282032302931))
REPRESENTATION_ITEM('')
);
#214=(
BOUNDED_CURVE()
B_SPLINE_CURVE(2,(#8284,#8285,#8286),.UNSPECIFIED.,.F.,.F.)
B_SPLINE_CURVE_WITH_KNOTS((3,3),(0.144988513094728,0.791574906712449),
 .UNSPECIFIED.)
CURVE()
GEOMETRIC_REPRESENTATION_ITEM()
RATIONAL_B_SPLINE_CURVE((1.09282032302755,1.26188021535082,1.09282032302931))
REPRESENTATION_ITEM('')
);
#215=(
BOUNDED_CURVE()
B_SPLINE_CURVE(2,(#8287,#8288,#8289),.UNSPECIFIED.,.F.,.F.)
B_SPLINE_CURVE_WITH_KNOTS((3,3),(0.144988513094728,0.791574906712449),
 .UNSPECIFIED.)
CURVE()
GEOMETRIC_REPRESENTATION_ITEM()
RATIONAL_B_SPLINE_CURVE((1.09282032302755,1.26188021535082,1.09282032302931))
REPRESENTATION_ITEM('')
);
#216=(
BOUNDED_CURVE()
B_SPLINE_CURVE(2,(#8296,#8297,#8298),.UNSPECIFIED.,.F.,.F.)
B_SPLINE_CURVE_WITH_KNOTS((3,3),(0.144988513094728,0.791574906712449),
 .UNSPECIFIED.)
CURVE()
GEOMETRIC_REPRESENTATION_ITEM()
RATIONAL_B_SPLINE_CURVE((1.09282032302755,1.26188021535082,1.09282032302931))
REPRESENTATION_ITEM('')
);
#217=(
BOUNDED_CURVE()
B_SPLINE_CURVE(2,(#8300,#8301,#8302),.UNSPECIFIED.,.F.,.F.)
B_SPLINE_CURVE_WITH_KNOTS((3,3),(0.144988513094727,0.791574906712449),
 .UNSPECIFIED.)
CURVE()
GEOMETRIC_REPRESENTATION_ITEM()
RATIONAL_B_SPLINE_CURVE((1.09282032302755,1.26188021535082,1.09282032302931))
REPRESENTATION_ITEM('')
);
#218=(
BOUNDED_CURVE()
B_SPLINE_CURVE(2,(#8304,#8305,#8306),.UNSPECIFIED.,.F.,.F.)
B_SPLINE_CURVE_WITH_KNOTS((3,3),(0.144988513094728,0.791574906712449),
 .UNSPECIFIED.)
CURVE()
GEOMETRIC_REPRESENTATION_ITEM()
RATIONAL_B_SPLINE_CURVE((1.09282032302755,1.26188021535082,1.09282032302931))
REPRESENTATION_ITEM('')
);
#219=(
BOUNDED_CURVE()
B_SPLINE_CURVE(2,(#8308,#8309,#8310),.UNSPECIFIED.,.F.,.F.)
B_SPLINE_CURVE_WITH_KNOTS((3,3),(0.144988513094728,0.791574906712449),
 .UNSPECIFIED.)
CURVE()
GEOMETRIC_REPRESENTATION_ITEM()
RATIONAL_B_SPLINE_CURVE((1.09282032302755,1.26188021535082,1.09282032302931))
REPRESENTATION_ITEM('')
);
#220=(
BOUNDED_CURVE()
B_SPLINE_CURVE(2,(#8312,#8313,#8314),.UNSPECIFIED.,.F.,.F.)
B_SPLINE_CURVE_WITH_KNOTS((3,3),(0.144988513094728,0.791574906712449),
 .UNSPECIFIED.)
CURVE()
GEOMETRIC_REPRESENTATION_ITEM()
RATIONAL_B_SPLINE_CURVE((1.09282032302755,1.26188021535082,1.09282032302931))
REPRESENTATION_ITEM('')
);
#221=(
BOUNDED_CURVE()
B_SPLINE_CURVE(2,(#8315,#8316,#8317),.UNSPECIFIED.,.F.,.F.)
B_SPLINE_CURVE_WITH_KNOTS((3,3),(0.144988513094727,0.791574906712449),
 .UNSPECIFIED.)
CURVE()
GEOMETRIC_REPRESENTATION_ITEM()
RATIONAL_B_SPLINE_CURVE((1.09282032302755,1.26188021535082,1.09282032302931))
REPRESENTATION_ITEM('')
);
#222=(
BOUNDED_CURVE()
B_SPLINE_CURVE(2,(#8377,#8378,#8379),.UNSPECIFIED.,.F.,.F.)
B_SPLINE_CURVE_WITH_KNOTS((3,3),(0.,0.154589948065443),.UNSPECIFIED.)
CURVE()
GEOMETRIC_REPRESENTATION_ITEM()
RATIONAL_B_SPLINE_CURVE((1.,1.03384052486396,1.))
REPRESENTATION_ITEM('')
);
#223=(
BOUNDED_CURVE()
B_SPLINE_CURVE(2,(#8383,#8384,#8385),.UNSPECIFIED.,.F.,.F.)
B_SPLINE_CURVE_WITH_KNOTS((3,3),(0.,0.154589948065443),.UNSPECIFIED.)
CURVE()
GEOMETRIC_REPRESENTATION_ITEM()
RATIONAL_B_SPLINE_CURVE((1.,1.03384052486396,1.))
REPRESENTATION_ITEM('')
);
#224=(
BOUNDED_CURVE()
B_SPLINE_CURVE(2,(#8405,#8406,#8407),.UNSPECIFIED.,.F.,.F.)
B_SPLINE_CURVE_WITH_KNOTS((3,3),(0.,0.154589948065443),.UNSPECIFIED.)
CURVE()
GEOMETRIC_REPRESENTATION_ITEM()
RATIONAL_B_SPLINE_CURVE((1.,1.03384052486396,1.))
REPRESENTATION_ITEM('')
);
#225=(
BOUNDED_CURVE()
B_SPLINE_CURVE(2,(#8412,#8413,#8414),.UNSPECIFIED.,.F.,.F.)
B_SPLINE_CURVE_WITH_KNOTS((3,3),(0.,0.154589948065443),.UNSPECIFIED.)
CURVE()
GEOMETRIC_REPRESENTATION_ITEM()
RATIONAL_B_SPLINE_CURVE((1.,1.03384052486396,1.))
REPRESENTATION_ITEM('')
);
#226=(
BOUNDED_CURVE()
B_SPLINE_CURVE(2,(#8838,#8839,#8840),.UNSPECIFIED.,.F.,.F.)
B_SPLINE_CURVE_WITH_KNOTS((3,3),(0.14973948338295,0.97160236658079),
 .UNSPECIFIED.)
CURVE()
GEOMETRIC_REPRESENTATION_ITEM()
RATIONAL_B_SPLINE_CURVE((1.07140024848292,1.23714644374248,1.07140024848292))
REPRESENTATION_ITEM('')
);
#227=(
BOUNDED_CURVE()
B_SPLINE_CURVE(2,(#8842,#8843,#8844),.UNSPECIFIED.,.F.,.F.)
B_SPLINE_CURVE_WITH_KNOTS((3,3),(0.14973948338295,0.97160236658079),
 .UNSPECIFIED.)
CURVE()
GEOMETRIC_REPRESENTATION_ITEM()
RATIONAL_B_SPLINE_CURVE((1.07140024848292,1.23714644374248,1.07140024848292))
REPRESENTATION_ITEM('')
);
#228=(
BOUNDED_CURVE()
B_SPLINE_CURVE(2,(#8846,#8847,#8848),.UNSPECIFIED.,.F.,.F.)
B_SPLINE_CURVE_WITH_KNOTS((3,3),(0.14973948338295,0.97160236658079),
 .UNSPECIFIED.)
CURVE()
GEOMETRIC_REPRESENTATION_ITEM()
RATIONAL_B_SPLINE_CURVE((1.07140024848292,1.23714644374248,1.07140024848292))
REPRESENTATION_ITEM('')
);
#229=(
BOUNDED_CURVE()
B_SPLINE_CURVE(2,(#8850,#8851,#8852),.UNSPECIFIED.,.F.,.F.)
B_SPLINE_CURVE_WITH_KNOTS((3,3),(0.149739483382949,0.971602366580789),
 .UNSPECIFIED.)
CURVE()
GEOMETRIC_REPRESENTATION_ITEM()
RATIONAL_B_SPLINE_CURVE((1.07140024848292,1.23714644374248,1.07140024848292))
REPRESENTATION_ITEM('')
);
#230=(
BOUNDED_CURVE()
B_SPLINE_CURVE(2,(#8854,#8855,#8856),.UNSPECIFIED.,.F.,.F.)
B_SPLINE_CURVE_WITH_KNOTS((3,3),(0.14973948338295,0.971602366580789),
 .UNSPECIFIED.)
CURVE()
GEOMETRIC_REPRESENTATION_ITEM()
RATIONAL_B_SPLINE_CURVE((1.07140024848292,1.23714644374248,1.07140024848292))
REPRESENTATION_ITEM('')
);
#231=(
BOUNDED_CURVE()
B_SPLINE_CURVE(2,(#8857,#8858,#8859),.UNSPECIFIED.,.F.,.F.)
B_SPLINE_CURVE_WITH_KNOTS((3,3),(0.14973948338295,0.97160236658079),
 .UNSPECIFIED.)
CURVE()
GEOMETRIC_REPRESENTATION_ITEM()
RATIONAL_B_SPLINE_CURVE((1.07140024848292,1.23714644374248,1.07140024848292))
REPRESENTATION_ITEM('')
);
#232=(
BOUNDED_CURVE()
B_SPLINE_CURVE(2,(#8890,#8891,#8892),.UNSPECIFIED.,.F.,.F.)
B_SPLINE_CURVE_WITH_KNOTS((3,3),(0.14973948338295,0.97160236658079),
 .UNSPECIFIED.)
CURVE()
GEOMETRIC_REPRESENTATION_ITEM()
RATIONAL_B_SPLINE_CURVE((1.07140024848292,1.23714644374248,1.07140024848292))
REPRESENTATION_ITEM('')
);
#233=(
BOUNDED_CURVE()
B_SPLINE_CURVE(2,(#8894,#8895,#8896),.UNSPECIFIED.,.F.,.F.)
B_SPLINE_CURVE_WITH_KNOTS((3,3),(0.14973948338295,0.971602366580789),
 .UNSPECIFIED.)
CURVE()
GEOMETRIC_REPRESENTATION_ITEM()
RATIONAL_B_SPLINE_CURVE((1.07140024848292,1.23714644374248,1.07140024848292))
REPRESENTATION_ITEM('')
);
#234=(
BOUNDED_CURVE()
B_SPLINE_CURVE(2,(#8901,#8902,#8903),.UNSPECIFIED.,.F.,.F.)
B_SPLINE_CURVE_WITH_KNOTS((3,3),(0.14973948338295,0.97160236658079),
 .UNSPECIFIED.)
CURVE()
GEOMETRIC_REPRESENTATION_ITEM()
RATIONAL_B_SPLINE_CURVE((1.07140024848292,1.23714644374248,1.07140024848292))
REPRESENTATION_ITEM('')
);
#235=(
BOUNDED_CURVE()
B_SPLINE_CURVE(2,(#8905,#8906,#8907),.UNSPECIFIED.,.F.,.F.)
B_SPLINE_CURVE_WITH_KNOTS((3,3),(0.14973948338295,0.97160236658079),
 .UNSPECIFIED.)
CURVE()
GEOMETRIC_REPRESENTATION_ITEM()
RATIONAL_B_SPLINE_CURVE((1.07140024848292,1.23714644374248,1.07140024848292))
REPRESENTATION_ITEM('')
);
#236=(
BOUNDED_CURVE()
B_SPLINE_CURVE(2,(#8909,#8910,#8911),.UNSPECIFIED.,.F.,.F.)
B_SPLINE_CURVE_WITH_KNOTS((3,3),(0.14973948338295,0.971602366580789),
 .UNSPECIFIED.)
CURVE()
GEOMETRIC_REPRESENTATION_ITEM()
RATIONAL_B_SPLINE_CURVE((1.07140024848292,1.23714644374248,1.07140024848292))
REPRESENTATION_ITEM('')
);
#237=(
BOUNDED_CURVE()
B_SPLINE_CURVE(2,(#8912,#8913,#8914),.UNSPECIFIED.,.F.,.F.)
B_SPLINE_CURVE_WITH_KNOTS((3,3),(0.14973948338295,0.97160236658079),
 .UNSPECIFIED.)
CURVE()
GEOMETRIC_REPRESENTATION_ITEM()
RATIONAL_B_SPLINE_CURVE((1.07140024848292,1.23714644374248,1.07140024848292))
REPRESENTATION_ITEM('')
);
#238=(
BOUNDED_CURVE()
B_SPLINE_CURVE(2,(#8921,#8922,#8923),.UNSPECIFIED.,.F.,.F.)
B_SPLINE_CURVE_WITH_KNOTS((3,3),(0.14973948338295,0.97160236658079),
 .UNSPECIFIED.)
CURVE()
GEOMETRIC_REPRESENTATION_ITEM()
RATIONAL_B_SPLINE_CURVE((1.07140024848292,1.23714644374248,1.07140024848292))
REPRESENTATION_ITEM('')
);
#239=(
BOUNDED_CURVE()
B_SPLINE_CURVE(2,(#8925,#8926,#8927),.UNSPECIFIED.,.F.,.F.)
B_SPLINE_CURVE_WITH_KNOTS((3,3),(0.14973948338295,0.97160236658079),
 .UNSPECIFIED.)
CURVE()
GEOMETRIC_REPRESENTATION_ITEM()
RATIONAL_B_SPLINE_CURVE((1.07140024848292,1.23714644374248,1.07140024848292))
REPRESENTATION_ITEM('')
);
#240=(
BOUNDED_CURVE()
B_SPLINE_CURVE(2,(#8929,#8930,#8931),.UNSPECIFIED.,.F.,.F.)
B_SPLINE_CURVE_WITH_KNOTS((3,3),(0.14973948338295,0.971602366580789),
 .UNSPECIFIED.)
CURVE()
GEOMETRIC_REPRESENTATION_ITEM()
RATIONAL_B_SPLINE_CURVE((1.07140024848292,1.23714644374248,1.07140024848292))
REPRESENTATION_ITEM('')
);
#241=(
BOUNDED_CURVE()
B_SPLINE_CURVE(2,(#8933,#8934,#8935),.UNSPECIFIED.,.F.,.F.)
B_SPLINE_CURVE_WITH_KNOTS((3,3),(0.14973948338295,0.97160236658079),
 .UNSPECIFIED.)
CURVE()
GEOMETRIC_REPRESENTATION_ITEM()
RATIONAL_B_SPLINE_CURVE((1.07140024848292,1.23714644374248,1.07140024848292))
REPRESENTATION_ITEM('')
);
#242=(
BOUNDED_CURVE()
B_SPLINE_CURVE(2,(#8937,#8938,#8939),.UNSPECIFIED.,.F.,.F.)
B_SPLINE_CURVE_WITH_KNOTS((3,3),(0.14973948338295,0.97160236658079),
 .UNSPECIFIED.)
CURVE()
GEOMETRIC_REPRESENTATION_ITEM()
RATIONAL_B_SPLINE_CURVE((1.07140024848292,1.23714644374248,1.07140024848292))
REPRESENTATION_ITEM('')
);
#243=(
BOUNDED_CURVE()
B_SPLINE_CURVE(2,(#8940,#8941,#8942),.UNSPECIFIED.,.F.,.F.)
B_SPLINE_CURVE_WITH_KNOTS((3,3),(0.14973948338295,0.971602366580789),
 .UNSPECIFIED.)
CURVE()
GEOMETRIC_REPRESENTATION_ITEM()
RATIONAL_B_SPLINE_CURVE((1.07140024848292,1.23714644374248,1.07140024848292))
REPRESENTATION_ITEM('')
);
#244=ORIENTED_CLOSED_SHELL('',*,#5172,.F.);
#245=ORIENTED_CLOSED_SHELL('',*,#5181,.F.);
#246=ORIENTED_CLOSED_SHELL('',*,#5185,.F.);
#247=BREP_WITH_VOIDS('Body1',#5173,(#244));
#248=BREP_WITH_VOIDS('Body1',#5182,(#245));
#249=BREP_WITH_VOIDS('Body1',#5186,(#246));
#250=CONICAL_SURFACE('',#5547,0.275,0.785398163397449);
#251=CONICAL_SURFACE('',#5570,0.4,0.785398163397448);
#252=CONICAL_SURFACE('',#5574,0.41,0.785398163397448);
#253=CONICAL_SURFACE('',#5578,0.26,0.463647609000806);
#254=CONICAL_SURFACE('',#5689,0.27,0.785398163397448);
#255=CONICAL_SURFACE('',#5692,0.576175134594813,1.0471975511966);
#256=CONICAL_SURFACE('',#5703,0.576175134594813,1.0471975511966);
#257=CONICAL_SURFACE('',#5705,0.576175134594813,1.0471975511966);
#258=CONICAL_SURFACE('',#5733,0.26,0.785398163397448);
#259=CONICAL_SURFACE('',#5746,0.26,0.785398163397448);
#260=CONICAL_SURFACE('',#5753,0.26,0.785398163397448);
#261=CONICAL_SURFACE('',#5767,0.625,0.785398163397448);
#262=CONICAL_SURFACE('',#5771,0.635,0.785398163397449);
#263=CONICAL_SURFACE('',#5775,0.41,0.463647609000806);
#264=CONICAL_SURFACE('',#5845,0.4,0.785398163397448);
#265=CONICAL_SURFACE('',#5849,0.41,0.785398163397448);
#266=CONICAL_SURFACE('',#5853,0.26,0.463647609000806);
#267=CONICAL_SURFACE('',#5905,0.36,0.785398163397451);
#268=CONICAL_SURFACE('',#5908,0.734027674973257,1.0471975511966);
#269=CONICAL_SURFACE('',#5919,0.734027674973257,1.0471975511966);
#270=CONICAL_SURFACE('',#5921,0.734027674973257,1.0471975511966);
#271=CONICAL_SURFACE('',#5944,0.475,0.785398163397448);
#272=CONICAL_SURFACE('',#5952,0.255,0.785398163397449);
#273=SHAPE_REPRESENTATION_RELATIONSHIP('SRR','None',#9396,#297);
#274=SHAPE_REPRESENTATION_RELATIONSHIP('SRR','None',#9397,#298);
#275=SHAPE_REPRESENTATION_RELATIONSHIP('SRR','None',#9398,#299);
#276=SHAPE_REPRESENTATION_RELATIONSHIP('SRR','None',#9399,#300);
#277=SHAPE_REPRESENTATION_RELATIONSHIP('SRR','None',#9400,#301);
#278=SHAPE_REPRESENTATION_RELATIONSHIP('SRR','None',#9401,#302);
#279=SHAPE_REPRESENTATION_RELATIONSHIP('SRR','None',#9402,#303);
#280=SHAPE_REPRESENTATION_RELATIONSHIP('SRR','None',#9403,#304);
#281=SHAPE_REPRESENTATION_RELATIONSHIP('SRR','None',#9404,#305);
#282=SHAPE_REPRESENTATION_RELATIONSHIP('SRR','None',#9405,#306);
#283=SHAPE_REPRESENTATION_RELATIONSHIP('SRR','None',#9406,#307);
#284=SHAPE_REPRESENTATION_RELATIONSHIP('SRR','None',#9407,#308);
#285=SHAPE_REPRESENTATION_RELATIONSHIP('SRR','None',#9409,#309);
#286=SHAPE_REPRESENTATION_RELATIONSHIP('SRR','None',#9410,#310);
#287=SHAPE_REPRESENTATION_RELATIONSHIP('SRR','None',#9411,#311);
#288=SHAPE_REPRESENTATION_RELATIONSHIP('SRR','None',#9413,#312);
#289=SHAPE_REPRESENTATION_RELATIONSHIP('SRR','None',#9415,#313);
#290=SHAPE_REPRESENTATION_RELATIONSHIP('SRR','None',#9416,#314);
#291=SHAPE_REPRESENTATION_RELATIONSHIP('SRR','None',#9417,#315);
#292=SHAPE_REPRESENTATION_RELATIONSHIP('SRR','None',#9418,#316);
#293=SHAPE_REPRESENTATION_RELATIONSHIP('SRR','None',#9419,#317);
#294=SHAPE_REPRESENTATION_RELATIONSHIP('SRR','None',#9420,#318);
#295=SHAPE_REPRESENTATION_RELATIONSHIP('SRR','None',#9421,#319);
#296=SHAPE_REPRESENTATION_RELATIONSHIP('SRR','None',#9422,#320);
#297=ADVANCED_BREP_SHAPE_REPRESENTATION('',(#345),#9258);
#298=ADVANCED_BREP_SHAPE_REPRESENTATION('',(#346),#9259);
#299=ADVANCED_BREP_SHAPE_REPRESENTATION('',(#347),#9260);
#300=ADVANCED_BREP_SHAPE_REPRESENTATION('',(#247),#9261);
#301=ADVANCED_BREP_SHAPE_REPRESENTATION('',(#348),#9262);
#302=ADVANCED_BREP_SHAPE_REPRESENTATION('',(#349),#9263);
#303=ADVANCED_BREP_SHAPE_REPRESENTATION('',(#350),#9264);
#304=ADVANCED_BREP_SHAPE_REPRESENTATION('',(#351),#9265);
#305=ADVANCED_BREP_SHAPE_REPRESENTATION('',(#352),#9266);
#306=ADVANCED_BREP_SHAPE_REPRESENTATION('',(#353),#9267);
#307=ADVANCED_BREP_SHAPE_REPRESENTATION('',(#354),#9268);
#308=ADVANCED_BREP_SHAPE_REPRESENTATION('',(#248),#9269);
#309=ADVANCED_BREP_SHAPE_REPRESENTATION('',(#355),#9271);
#310=ADVANCED_BREP_SHAPE_REPRESENTATION('',(#356),#9272);
#311=ADVANCED_BREP_SHAPE_REPRESENTATION('',(#249),#9273);
#312=ADVANCED_BREP_SHAPE_REPRESENTATION('',(#357),#9275);
#313=ADVANCED_BREP_SHAPE_REPRESENTATION('',(#358),#9277);
#314=ADVANCED_BREP_SHAPE_REPRESENTATION('',(#359),#9278);
#315=ADVANCED_BREP_SHAPE_REPRESENTATION('',(#360),#9279);
#316=ADVANCED_BREP_SHAPE_REPRESENTATION('',(#361),#9280);
#317=ADVANCED_BREP_SHAPE_REPRESENTATION('',(#362),#9281);
#318=ADVANCED_BREP_SHAPE_REPRESENTATION('',(#363),#9282);
#319=ADVANCED_BREP_SHAPE_REPRESENTATION('',(#364),#9283);
#320=ADVANCED_BREP_SHAPE_REPRESENTATION('',(#365),#9284);
#321=STYLED_ITEM('',(#9591),#345);
#322=STYLED_ITEM('',(#9619),#346);
#323=STYLED_ITEM('',(#9619),#347);
#324=STYLED_ITEM('',(#9619),#247);
#325=STYLED_ITEM('',(#9598),#348);
#326=STYLED_ITEM('',(#9619),#349);
#327=STYLED_ITEM('',(#9619),#350);
#328=STYLED_ITEM('',(#9619),#351);
#329=STYLED_ITEM('',(#9626),#352);
#330=STYLED_ITEM('',(#9612),#353);
#331=STYLED_ITEM('',(#9612),#354);
#332=STYLED_ITEM('',(#9619),#248);
#333=STYLED_ITEM('',(#9598),#355);
#334=STYLED_ITEM('',(#9605),#356);
#335=STYLED_ITEM('',(#9619),#249);
#336=STYLED_ITEM('',(#9626),#357);
#337=STYLED_ITEM('',(#9598),#358);
#338=STYLED_ITEM('',(#9619),#359);
#339=STYLED_ITEM('',(#9619),#360);
#340=STYLED_ITEM('',(#9626),#361);
#341=STYLED_ITEM('',(#9612),#362);
#342=STYLED_ITEM('',(#9619),#363);
#343=STYLED_ITEM('',(#9626),#364);
#344=STYLED_ITEM('',(#9612),#365);
#345=MANIFOLD_SOLID_BREP('Body1',#5169);
#346=MANIFOLD_SOLID_BREP('Body1',#5170);
#347=MANIFOLD_SOLID_BREP('Body1',#5171);
#348=MANIFOLD_SOLID_BREP('Body1',#5174);
#349=MANIFOLD_SOLID_BREP('Body1',#5175);
#350=MANIFOLD_SOLID_BREP('Body1',#5176);
#351=MANIFOLD_SOLID_BREP('Body1',#5177);
#352=MANIFOLD_SOLID_BREP('Body1',#5178);
#353=MANIFOLD_SOLID_BREP('Body1',#5179);
#354=MANIFOLD_SOLID_BREP('Body1',#5180);
#355=MANIFOLD_SOLID_BREP('Body1',#5183);
#356=MANIFOLD_SOLID_BREP('Body1',#5184);
#357=MANIFOLD_SOLID_BREP('Body1',#5187);
#358=MANIFOLD_SOLID_BREP('Body1',#5188);
#359=MANIFOLD_SOLID_BREP('Body1',#5189);
#360=MANIFOLD_SOLID_BREP('Body1',#5190);
#361=MANIFOLD_SOLID_BREP('Body1',#5191);
#362=MANIFOLD_SOLID_BREP('Body1',#5192);
#363=MANIFOLD_SOLID_BREP('Body1',#5193);
#364=MANIFOLD_SOLID_BREP('Body1',#5194);
#365=MANIFOLD_SOLID_BREP('Body1',#5195);
#366=FACE_BOUND('',#977,.T.);
#367=FACE_BOUND('',#978,.T.);
#368=FACE_BOUND('',#979,.T.);
#369=FACE_BOUND('',#980,.T.);
#370=FACE_BOUND('',#981,.T.);
#371=FACE_BOUND('',#987,.T.);
#372=FACE_BOUND('',#989,.T.);
#373=FACE_BOUND('',#995,.T.);
#374=FACE_BOUND('',#1000,.T.);
#375=FACE_BOUND('',#1002,.T.);
#376=FACE_BOUND('',#1007,.T.);
#377=FACE_BOUND('',#1012,.T.);
#378=FACE_BOUND('',#1013,.T.);
#379=FACE_BOUND('',#1017,.T.);
#380=FACE_BOUND('',#1018,.T.);
#381=FACE_BOUND('',#1027,.T.);
#382=FACE_BOUND('',#1034,.T.);
#383=FACE_BOUND('',#1038,.T.);
#384=FACE_BOUND('',#1039,.T.);
#385=FACE_BOUND('',#1047,.T.);
#386=FACE_BOUND('',#1050,.T.);
#387=FACE_BOUND('',#1065,.T.);
#388=FACE_BOUND('',#1098,.T.);
#389=FACE_BOUND('',#1099,.T.);
#390=FACE_BOUND('',#1100,.T.);
#391=FACE_BOUND('',#1101,.T.);
#392=FACE_BOUND('',#1102,.T.);
#393=FACE_BOUND('',#1103,.T.);
#394=FACE_BOUND('',#1104,.T.);
#395=FACE_BOUND('',#1105,.T.);
#396=FACE_BOUND('',#1106,.T.);
#397=FACE_BOUND('',#1107,.T.);
#398=FACE_BOUND('',#1108,.T.);
#399=FACE_BOUND('',#1109,.T.);
#400=FACE_BOUND('',#1110,.T.);
#401=FACE_BOUND('',#1111,.T.);
#402=FACE_BOUND('',#1112,.T.);
#403=FACE_BOUND('',#1113,.T.);
#404=FACE_BOUND('',#1114,.T.);
#405=FACE_BOUND('',#1115,.T.);
#406=FACE_BOUND('',#1116,.T.);
#407=FACE_BOUND('',#1117,.T.);
#408=FACE_BOUND('',#1118,.T.);
#409=FACE_BOUND('',#1119,.T.);
#410=FACE_BOUND('',#1120,.T.);
#411=FACE_BOUND('',#1121,.T.);
#412=FACE_BOUND('',#1122,.T.);
#413=FACE_BOUND('',#1123,.T.);
#414=FACE_BOUND('',#1124,.T.);
#415=FACE_BOUND('',#1125,.T.);
#416=FACE_BOUND('',#1128,.T.);
#417=FACE_BOUND('',#1129,.T.);
#418=FACE_BOUND('',#1130,.T.);
#419=FACE_BOUND('',#1131,.T.);
#420=FACE_BOUND('',#1132,.T.);
#421=FACE_BOUND('',#1133,.T.);
#422=FACE_BOUND('',#1134,.T.);
#423=FACE_BOUND('',#1135,.T.);
#424=FACE_BOUND('',#1136,.T.);
#425=FACE_BOUND('',#1137,.T.);
#426=FACE_BOUND('',#1138,.T.);
#427=FACE_BOUND('',#1139,.T.);
#428=FACE_BOUND('',#1140,.T.);
#429=FACE_BOUND('',#1141,.T.);
#430=FACE_BOUND('',#1142,.T.);
#431=FACE_BOUND('',#1143,.T.);
#432=FACE_BOUND('',#1144,.T.);
#433=FACE_BOUND('',#1145,.T.);
#434=FACE_BOUND('',#1146,.T.);
#435=FACE_BOUND('',#1147,.T.);
#436=FACE_BOUND('',#1148,.T.);
#437=FACE_BOUND('',#1149,.T.);
#438=FACE_BOUND('',#1150,.T.);
#439=FACE_BOUND('',#1151,.T.);
#440=FACE_BOUND('',#1152,.T.);
#441=FACE_BOUND('',#1153,.T.);
#442=FACE_BOUND('',#1154,.T.);
#443=FACE_BOUND('',#1155,.T.);
#444=FACE_BOUND('',#1162,.T.);
#445=FACE_BOUND('',#1163,.T.);
#446=FACE_BOUND('',#1166,.T.);
#447=FACE_BOUND('',#1167,.T.);
#448=FACE_BOUND('',#1182,.T.);
#449=FACE_BOUND('',#1193,.T.);
#450=FACE_BOUND('',#1195,.T.);
#451=FACE_BOUND('',#1200,.T.);
#452=FACE_BOUND('',#1229,.T.);
#453=FACE_BOUND('',#1236,.T.);
#454=FACE_BOUND('',#1239,.T.);
#455=FACE_BOUND('',#1245,.T.);
#456=FACE_BOUND('',#1248,.T.);
#457=FACE_BOUND('',#1254,.T.);
#458=FACE_BOUND('',#1255,.T.);
#459=FACE_BOUND('',#1257,.T.);
#460=FACE_BOUND('',#1259,.T.);
#461=FACE_BOUND('',#1262,.T.);
#462=FACE_BOUND('',#1264,.T.);
#463=FACE_BOUND('',#1268,.T.);
#464=FACE_BOUND('',#1273,.T.);
#465=FACE_BOUND('',#1289,.T.);
#466=FACE_BOUND('',#1297,.T.);
#467=FACE_BOUND('',#1298,.T.);
#468=FACE_BOUND('',#1302,.T.);
#469=FACE_BOUND('',#1303,.T.);
#470=FACE_BOUND('',#1310,.T.);
#471=FACE_BOUND('',#1313,.T.);
#472=FACE_BOUND('',#1316,.T.);
#473=FACE_BOUND('',#1319,.T.);
#474=FACE_BOUND('',#1322,.T.);
#475=FACE_BOUND('',#1325,.T.);
#476=FACE_BOUND('',#1338,.T.);
#477=FACE_BOUND('',#1349,.T.);
#478=FACE_BOUND('',#1351,.T.);
#479=FACE_BOUND('',#1360,.T.);
#480=FACE_BOUND('',#1362,.T.);
#481=FACE_BOUND('',#1368,.T.);
#482=FACE_BOUND('',#1370,.T.);
#483=FACE_BOUND('',#1374,.T.);
#484=FACE_BOUND('',#1376,.T.);
#485=FACE_BOUND('',#1378,.T.);
#486=PLANE('',#5469);
#487=PLANE('',#5470);
#488=PLANE('',#5471);
#489=PLANE('',#5472);
#490=PLANE('',#5473);
#491=PLANE('',#5474);
#492=PLANE('',#5475);
#493=PLANE('',#5476);
#494=PLANE('',#5486);
#495=PLANE('',#5487);
#496=PLANE('',#5488);
#497=PLANE('',#5489);
#498=PLANE('',#5490);
#499=PLANE('',#5497);
#500=PLANE('',#5498);
#501=PLANE('',#5499);
#502=PLANE('',#5500);
#503=PLANE('',#5501);
#504=PLANE('',#5502);
#505=PLANE('',#5503);
#506=PLANE('',#5504);
#507=PLANE('',#5505);
#508=PLANE('',#5506);
#509=PLANE('',#5507);
#510=PLANE('',#5508);
#511=PLANE('',#5509);
#512=PLANE('',#5510);
#513=PLANE('',#5515);
#514=PLANE('',#5516);
#515=PLANE('',#5523);
#516=PLANE('',#5527);
#517=PLANE('',#5528);
#518=PLANE('',#5529);
#519=PLANE('',#5530);
#520=PLANE('',#5531);
#521=PLANE('',#5535);
#522=PLANE('',#5536);
#523=PLANE('',#5537);
#524=PLANE('',#5538);
#525=PLANE('',#5539);
#526=PLANE('',#5540);
#527=PLANE('',#5541);
#528=PLANE('',#5542);
#529=PLANE('',#5543);
#530=PLANE('',#5544);
#531=PLANE('',#5545);
#532=PLANE('',#5552);
#533=PLANE('',#5556);
#534=PLANE('',#5558);
#535=PLANE('',#5559);
#536=PLANE('',#5560);
#537=PLANE('',#5561);
#538=PLANE('',#5562);
#539=PLANE('',#5563);
#540=PLANE('',#5564);
#541=PLANE('',#5565);
#542=PLANE('',#5566);
#543=PLANE('',#5568);
#544=PLANE('',#5576);
#545=PLANE('',#5666);
#546=PLANE('',#5667);
#547=PLANE('',#5668);
#548=PLANE('',#5669);
#549=PLANE('',#5670);
#550=PLANE('',#5671);
#551=PLANE('',#5679);
#552=PLANE('',#5680);
#553=PLANE('',#5681);
#554=PLANE('',#5682);
#555=PLANE('',#5683);
#556=PLANE('',#5684);
#557=PLANE('',#5691);
#558=PLANE('',#5694);
#559=PLANE('',#5695);
#560=PLANE('',#5696);
#561=PLANE('',#5697);
#562=PLANE('',#5698);
#563=PLANE('',#5699);
#564=PLANE('',#5700);
#565=PLANE('',#5701);
#566=PLANE('',#5707);
#567=PLANE('',#5708);
#568=PLANE('',#5709);
#569=PLANE('',#5713);
#570=PLANE('',#5714);
#571=PLANE('',#5715);
#572=PLANE('',#5716);
#573=PLANE('',#5717);
#574=PLANE('',#5722);
#575=PLANE('',#5726);
#576=PLANE('',#5727);
#577=PLANE('',#5735);
#578=PLANE('',#5737);
#579=PLANE('',#5739);
#580=PLANE('',#5748);
#581=PLANE('',#5749);
#582=PLANE('',#5750);
#583=PLANE('',#5755);
#584=PLANE('',#5756);
#585=PLANE('',#5757);
#586=PLANE('',#5758);
#587=PLANE('',#5759);
#588=PLANE('',#5760);
#589=PLANE('',#5761);
#590=PLANE('',#5762);
#591=PLANE('',#5763);
#592=PLANE('',#5765);
#593=PLANE('',#5773);
#594=PLANE('',#5789);
#595=PLANE('',#5791);
#596=PLANE('',#5792);
#597=PLANE('',#5794);
#598=PLANE('',#5801);
#599=PLANE('',#5802);
#600=PLANE('',#5803);
#601=PLANE('',#5804);
#602=PLANE('',#5805);
#603=PLANE('',#5807);
#604=PLANE('',#5808);
#605=PLANE('',#5810);
#606=PLANE('',#5814);
#607=PLANE('',#5815);
#608=PLANE('',#5816);
#609=PLANE('',#5817);
#610=PLANE('',#5818);
#611=PLANE('',#5819);
#612=PLANE('',#5820);
#613=PLANE('',#5821);
#614=PLANE('',#5826);
#615=PLANE('',#5830);
#616=PLANE('',#5831);
#617=PLANE('',#5833);
#618=PLANE('',#5834);
#619=PLANE('',#5835);
#620=PLANE('',#5836);
#621=PLANE('',#5837);
#622=PLANE('',#5838);
#623=PLANE('',#5839);
#624=PLANE('',#5840);
#625=PLANE('',#5841);
#626=PLANE('',#5843);
#627=PLANE('',#5851);
#628=PLANE('',#5867);
#629=PLANE('',#5868);
#630=PLANE('',#5870);
#631=PLANE('',#5873);
#632=PLANE('',#5880);
#633=PLANE('',#5887);
#634=PLANE('',#5888);
#635=PLANE('',#5889);
#636=PLANE('',#5890);
#637=PLANE('',#5891);
#638=PLANE('',#5892);
#639=PLANE('',#5894);
#640=PLANE('',#5895);
#641=PLANE('',#5896);
#642=PLANE('',#5897);
#643=PLANE('',#5900);
#644=PLANE('',#5907);
#645=PLANE('',#5910);
#646=PLANE('',#5911);
#647=PLANE('',#5912);
#648=PLANE('',#5913);
#649=PLANE('',#5914);
#650=PLANE('',#5915);
#651=PLANE('',#5916);
#652=PLANE('',#5917);
#653=PLANE('',#5923);
#654=PLANE('',#5924);
#655=PLANE('',#5925);
#656=PLANE('',#5929);
#657=PLANE('',#5930);
#658=PLANE('',#5931);
#659=PLANE('',#5932);
#660=PLANE('',#5933);
#661=PLANE('',#5938);
#662=PLANE('',#5939);
#663=PLANE('',#5942);
#664=PLANE('',#5948);
#665=PLANE('',#5954);
#666=PLANE('',#5962);
#667=PLANE('',#5963);
#668=PLANE('',#5971);
#669=PLANE('',#5972);
#670=PLANE('',#5977);
#671=PLANE('',#5979);
#672=PLANE('',#5983);
#673=FACE_OUTER_BOUND('',#968,.T.);
#674=FACE_OUTER_BOUND('',#969,.T.);
#675=FACE_OUTER_BOUND('',#970,.T.);
#676=FACE_OUTER_BOUND('',#971,.T.);
#677=FACE_OUTER_BOUND('',#972,.T.);
#678=FACE_OUTER_BOUND('',#973,.T.);
#679=FACE_OUTER_BOUND('',#974,.T.);
#680=FACE_OUTER_BOUND('',#975,.T.);
#681=FACE_OUTER_BOUND('',#976,.T.);
#682=FACE_OUTER_BOUND('',#982,.T.);
#683=FACE_OUTER_BOUND('',#983,.T.);
#684=FACE_OUTER_BOUND('',#984,.T.);
#685=FACE_OUTER_BOUND('',#985,.T.);
#686=FACE_OUTER_BOUND('',#986,.T.);
#687=FACE_OUTER_BOUND('',#988,.T.);
#688=FACE_OUTER_BOUND('',#990,.T.);
#689=FACE_OUTER_BOUND('',#991,.T.);
#690=FACE_OUTER_BOUND('',#992,.T.);
#691=FACE_OUTER_BOUND('',#993,.T.);
#692=FACE_OUTER_BOUND('',#994,.T.);
#693=FACE_OUTER_BOUND('',#996,.T.);
#694=FACE_OUTER_BOUND('',#997,.T.);
#695=FACE_OUTER_BOUND('',#998,.T.);
#696=FACE_OUTER_BOUND('',#999,.T.);
#697=FACE_OUTER_BOUND('',#1001,.T.);
#698=FACE_OUTER_BOUND('',#1003,.T.);
#699=FACE_OUTER_BOUND('',#1004,.T.);
#700=FACE_OUTER_BOUND('',#1005,.T.);
#701=FACE_OUTER_BOUND('',#1006,.T.);
#702=FACE_OUTER_BOUND('',#1008,.T.);
#703=FACE_OUTER_BOUND('',#1009,.T.);
#704=FACE_OUTER_BOUND('',#1010,.T.);
#705=FACE_OUTER_BOUND('',#1011,.T.);
#706=FACE_OUTER_BOUND('',#1014,.T.);
#707=FACE_OUTER_BOUND('',#1015,.T.);
#708=FACE_OUTER_BOUND('',#1016,.T.);
#709=FACE_OUTER_BOUND('',#1019,.T.);
#710=FACE_OUTER_BOUND('',#1020,.T.);
#711=FACE_OUTER_BOUND('',#1021,.T.);
#712=FACE_OUTER_BOUND('',#1022,.T.);
#713=FACE_OUTER_BOUND('',#1023,.T.);
#714=FACE_OUTER_BOUND('',#1024,.T.);
#715=FACE_OUTER_BOUND('',#1025,.T.);
#716=FACE_OUTER_BOUND('',#1026,.T.);
#717=FACE_OUTER_BOUND('',#1028,.T.);
#718=FACE_OUTER_BOUND('',#1029,.T.);
#719=FACE_OUTER_BOUND('',#1030,.T.);
#720=FACE_OUTER_BOUND('',#1031,.T.);
#721=FACE_OUTER_BOUND('',#1032,.T.);
#722=FACE_OUTER_BOUND('',#1033,.T.);
#723=FACE_OUTER_BOUND('',#1035,.T.);
#724=FACE_OUTER_BOUND('',#1036,.T.);
#725=FACE_OUTER_BOUND('',#1037,.T.);
#726=FACE_OUTER_BOUND('',#1040,.T.);
#727=FACE_OUTER_BOUND('',#1041,.T.);
#728=FACE_OUTER_BOUND('',#1042,.T.);
#729=FACE_OUTER_BOUND('',#1043,.T.);
#730=FACE_OUTER_BOUND('',#1044,.T.);
#731=FACE_OUTER_BOUND('',#1045,.T.);
#732=FACE_OUTER_BOUND('',#1046,.T.);
#733=FACE_OUTER_BOUND('',#1048,.T.);
#734=FACE_OUTER_BOUND('',#1049,.T.);
#735=FACE_OUTER_BOUND('',#1051,.T.);
#736=FACE_OUTER_BOUND('',#1052,.T.);
#737=FACE_OUTER_BOUND('',#1053,.T.);
#738=FACE_OUTER_BOUND('',#1054,.T.);
#739=FACE_OUTER_BOUND('',#1055,.T.);
#740=FACE_OUTER_BOUND('',#1056,.T.);
#741=FACE_OUTER_BOUND('',#1057,.T.);
#742=FACE_OUTER_BOUND('',#1058,.T.);
#743=FACE_OUTER_BOUND('',#1059,.T.);
#744=FACE_OUTER_BOUND('',#1060,.T.);
#745=FACE_OUTER_BOUND('',#1061,.T.);
#746=FACE_OUTER_BOUND('',#1062,.T.);
#747=FACE_OUTER_BOUND('',#1063,.T.);
#748=FACE_OUTER_BOUND('',#1064,.T.);
#749=FACE_OUTER_BOUND('',#1066,.T.);
#750=FACE_OUTER_BOUND('',#1067,.T.);
#751=FACE_OUTER_BOUND('',#1068,.T.);
#752=FACE_OUTER_BOUND('',#1069,.T.);
#753=FACE_OUTER_BOUND('',#1070,.T.);
#754=FACE_OUTER_BOUND('',#1071,.T.);
#755=FACE_OUTER_BOUND('',#1072,.T.);
#756=FACE_OUTER_BOUND('',#1073,.T.);
#757=FACE_OUTER_BOUND('',#1074,.T.);
#758=FACE_OUTER_BOUND('',#1075,.T.);
#759=FACE_OUTER_BOUND('',#1076,.T.);
#760=FACE_OUTER_BOUND('',#1077,.T.);
#761=FACE_OUTER_BOUND('',#1078,.T.);
#762=FACE_OUTER_BOUND('',#1079,.T.);
#763=FACE_OUTER_BOUND('',#1080,.T.);
#764=FACE_OUTER_BOUND('',#1081,.T.);
#765=FACE_OUTER_BOUND('',#1082,.T.);
#766=FACE_OUTER_BOUND('',#1083,.T.);
#767=FACE_OUTER_BOUND('',#1084,.T.);
#768=FACE_OUTER_BOUND('',#1085,.T.);
#769=FACE_OUTER_BOUND('',#1086,.T.);
#770=FACE_OUTER_BOUND('',#1087,.T.);
#771=FACE_OUTER_BOUND('',#1088,.T.);
#772=FACE_OUTER_BOUND('',#1089,.T.);
#773=FACE_OUTER_BOUND('',#1090,.T.);
#774=FACE_OUTER_BOUND('',#1091,.T.);
#775=FACE_OUTER_BOUND('',#1092,.T.);
#776=FACE_OUTER_BOUND('',#1093,.T.);
#777=FACE_OUTER_BOUND('',#1094,.T.);
#778=FACE_OUTER_BOUND('',#1095,.T.);
#779=FACE_OUTER_BOUND('',#1096,.T.);
#780=FACE_OUTER_BOUND('',#1097,.T.);
#781=FACE_OUTER_BOUND('',#1126,.T.);
#782=FACE_OUTER_BOUND('',#1127,.T.);
#783=FACE_OUTER_BOUND('',#1156,.T.);
#784=FACE_OUTER_BOUND('',#1157,.T.);
#785=FACE_OUTER_BOUND('',#1158,.T.);
#786=FACE_OUTER_BOUND('',#1159,.T.);
#787=FACE_OUTER_BOUND('',#1160,.T.);
#788=FACE_OUTER_BOUND('',#1161,.T.);
#789=FACE_OUTER_BOUND('',#1164,.T.);
#790=FACE_OUTER_BOUND('',#1165,.T.);
#791=FACE_OUTER_BOUND('',#1168,.T.);
#792=FACE_OUTER_BOUND('',#1169,.T.);
#793=FACE_OUTER_BOUND('',#1170,.T.);
#794=FACE_OUTER_BOUND('',#1171,.T.);
#795=FACE_OUTER_BOUND('',#1172,.T.);
#796=FACE_OUTER_BOUND('',#1173,.T.);
#797=FACE_OUTER_BOUND('',#1174,.T.);
#798=FACE_OUTER_BOUND('',#1175,.T.);
#799=FACE_OUTER_BOUND('',#1176,.T.);
#800=FACE_OUTER_BOUND('',#1177,.T.);
#801=FACE_OUTER_BOUND('',#1178,.T.);
#802=FACE_OUTER_BOUND('',#1179,.T.);
#803=FACE_OUTER_BOUND('',#1180,.T.);
#804=FACE_OUTER_BOUND('',#1181,.T.);
#805=FACE_OUTER_BOUND('',#1183,.T.);
#806=FACE_OUTER_BOUND('',#1184,.T.);
#807=FACE_OUTER_BOUND('',#1185,.T.);
#808=FACE_OUTER_BOUND('',#1186,.T.);
#809=FACE_OUTER_BOUND('',#1187,.T.);
#810=FACE_OUTER_BOUND('',#1188,.T.);
#811=FACE_OUTER_BOUND('',#1189,.T.);
#812=FACE_OUTER_BOUND('',#1190,.T.);
#813=FACE_OUTER_BOUND('',#1191,.T.);
#814=FACE_OUTER_BOUND('',#1192,.T.);
#815=FACE_OUTER_BOUND('',#1194,.T.);
#816=FACE_OUTER_BOUND('',#1196,.T.);
#817=FACE_OUTER_BOUND('',#1197,.T.);
#818=FACE_OUTER_BOUND('',#1198,.T.);
#819=FACE_OUTER_BOUND('',#1199,.T.);
#820=FACE_OUTER_BOUND('',#1201,.T.);
#821=FACE_OUTER_BOUND('',#1202,.T.);
#822=FACE_OUTER_BOUND('',#1203,.T.);
#823=FACE_OUTER_BOUND('',#1204,.T.);
#824=FACE_OUTER_BOUND('',#1205,.T.);
#825=FACE_OUTER_BOUND('',#1206,.T.);
#826=FACE_OUTER_BOUND('',#1207,.T.);
#827=FACE_OUTER_BOUND('',#1208,.T.);
#828=FACE_OUTER_BOUND('',#1209,.T.);
#829=FACE_OUTER_BOUND('',#1210,.T.);
#830=FACE_OUTER_BOUND('',#1211,.T.);
#831=FACE_OUTER_BOUND('',#1212,.T.);
#832=FACE_OUTER_BOUND('',#1213,.T.);
#833=FACE_OUTER_BOUND('',#1214,.T.);
#834=FACE_OUTER_BOUND('',#1215,.T.);
#835=FACE_OUTER_BOUND('',#1216,.T.);
#836=FACE_OUTER_BOUND('',#1217,.T.);
#837=FACE_OUTER_BOUND('',#1218,.T.);
#838=FACE_OUTER_BOUND('',#1219,.T.);
#839=FACE_OUTER_BOUND('',#1220,.T.);
#840=FACE_OUTER_BOUND('',#1221,.T.);
#841=FACE_OUTER_BOUND('',#1222,.T.);
#842=FACE_OUTER_BOUND('',#1223,.T.);
#843=FACE_OUTER_BOUND('',#1224,.T.);
#844=FACE_OUTER_BOUND('',#1225,.T.);
#845=FACE_OUTER_BOUND('',#1226,.T.);
#846=FACE_OUTER_BOUND('',#1227,.T.);
#847=FACE_OUTER_BOUND('',#1228,.T.);
#848=FACE_OUTER_BOUND('',#1230,.T.);
#849=FACE_OUTER_BOUND('',#1231,.T.);
#850=FACE_OUTER_BOUND('',#1232,.T.);
#851=FACE_OUTER_BOUND('',#1233,.T.);
#852=FACE_OUTER_BOUND('',#1234,.T.);
#853=FACE_OUTER_BOUND('',#1235,.T.);
#854=FACE_OUTER_BOUND('',#1237,.T.);
#855=FACE_OUTER_BOUND('',#1238,.T.);
#856=FACE_OUTER_BOUND('',#1240,.T.);
#857=FACE_OUTER_BOUND('',#1241,.T.);
#858=FACE_OUTER_BOUND('',#1242,.T.);
#859=FACE_OUTER_BOUND('',#1243,.T.);
#860=FACE_OUTER_BOUND('',#1244,.T.);
#861=FACE_OUTER_BOUND('',#1246,.T.);
#862=FACE_OUTER_BOUND('',#1247,.T.);
#863=FACE_OUTER_BOUND('',#1249,.T.);
#864=FACE_OUTER_BOUND('',#1250,.T.);
#865=FACE_OUTER_BOUND('',#1251,.T.);
#866=FACE_OUTER_BOUND('',#1252,.T.);
#867=FACE_OUTER_BOUND('',#1253,.T.);
#868=FACE_OUTER_BOUND('',#1256,.T.);
#869=FACE_OUTER_BOUND('',#1258,.T.);
#870=FACE_OUTER_BOUND('',#1260,.T.);
#871=FACE_OUTER_BOUND('',#1261,.T.);
#872=FACE_OUTER_BOUND('',#1263,.T.);
#873=FACE_OUTER_BOUND('',#1265,.T.);
#874=FACE_OUTER_BOUND('',#1266,.T.);
#875=FACE_OUTER_BOUND('',#1267,.T.);
#876=FACE_OUTER_BOUND('',#1269,.T.);
#877=FACE_OUTER_BOUND('',#1270,.T.);
#878=FACE_OUTER_BOUND('',#1271,.T.);
#879=FACE_OUTER_BOUND('',#1272,.T.);
#880=FACE_OUTER_BOUND('',#1274,.T.);
#881=FACE_OUTER_BOUND('',#1275,.T.);
#882=FACE_OUTER_BOUND('',#1276,.T.);
#883=FACE_OUTER_BOUND('',#1277,.T.);
#884=FACE_OUTER_BOUND('',#1278,.T.);
#885=FACE_OUTER_BOUND('',#1279,.T.);
#886=FACE_OUTER_BOUND('',#1280,.T.);
#887=FACE_OUTER_BOUND('',#1281,.T.);
#888=FACE_OUTER_BOUND('',#1282,.T.);
#889=FACE_OUTER_BOUND('',#1283,.T.);
#890=FACE_OUTER_BOUND('',#1284,.T.);
#891=FACE_OUTER_BOUND('',#1285,.T.);
#892=FACE_OUTER_BOUND('',#1286,.T.);
#893=FACE_OUTER_BOUND('',#1287,.T.);
#894=FACE_OUTER_BOUND('',#1288,.T.);
#895=FACE_OUTER_BOUND('',#1290,.T.);
#896=FACE_OUTER_BOUND('',#1291,.T.);
#897=FACE_OUTER_BOUND('',#1292,.T.);
#898=FACE_OUTER_BOUND('',#1293,.T.);
#899=FACE_OUTER_BOUND('',#1294,.T.);
#900=FACE_OUTER_BOUND('',#1295,.T.);
#901=FACE_OUTER_BOUND('',#1296,.T.);
#902=FACE_OUTER_BOUND('',#1299,.T.);
#903=FACE_OUTER_BOUND('',#1300,.T.);
#904=FACE_OUTER_BOUND('',#1301,.T.);
#905=FACE_OUTER_BOUND('',#1304,.T.);
#906=FACE_OUTER_BOUND('',#1305,.T.);
#907=FACE_OUTER_BOUND('',#1306,.T.);
#908=FACE_OUTER_BOUND('',#1307,.T.);
#909=FACE_OUTER_BOUND('',#1308,.T.);
#910=FACE_OUTER_BOUND('',#1309,.T.);
#911=FACE_OUTER_BOUND('',#1311,.T.);
#912=FACE_OUTER_BOUND('',#1312,.T.);
#913=FACE_OUTER_BOUND('',#1314,.T.);
#914=FACE_OUTER_BOUND('',#1315,.T.);
#915=FACE_OUTER_BOUND('',#1317,.T.);
#916=FACE_OUTER_BOUND('',#1318,.T.);
#917=FACE_OUTER_BOUND('',#1320,.T.);
#918=FACE_OUTER_BOUND('',#1321,.T.);
#919=FACE_OUTER_BOUND('',#1323,.T.);
#920=FACE_OUTER_BOUND('',#1324,.T.);
#921=FACE_OUTER_BOUND('',#1326,.T.);
#922=FACE_OUTER_BOUND('',#1327,.T.);
#923=FACE_OUTER_BOUND('',#1328,.T.);
#924=FACE_OUTER_BOUND('',#1329,.T.);
#925=FACE_OUTER_BOUND('',#1330,.T.);
#926=FACE_OUTER_BOUND('',#1331,.T.);
#927=FACE_OUTER_BOUND('',#1332,.T.);
#928=FACE_OUTER_BOUND('',#1333,.T.);
#929=FACE_OUTER_BOUND('',#1334,.T.);
#930=FACE_OUTER_BOUND('',#1335,.T.);
#931=FACE_OUTER_BOUND('',#1336,.T.);
#932=FACE_OUTER_BOUND('',#1337,.T.);
#933=FACE_OUTER_BOUND('',#1339,.T.);
#934=FACE_OUTER_BOUND('',#1340,.T.);
#935=FACE_OUTER_BOUND('',#1341,.T.);
#936=FACE_OUTER_BOUND('',#1342,.T.);
#937=FACE_OUTER_BOUND('',#1343,.T.);
#938=FACE_OUTER_BOUND('',#1344,.T.);
#939=FACE_OUTER_BOUND('',#1345,.T.);
#940=FACE_OUTER_BOUND('',#1346,.T.);
#941=FACE_OUTER_BOUND('',#1347,.T.);
#942=FACE_OUTER_BOUND('',#1348,.T.);
#943=FACE_OUTER_BOUND('',#1350,.T.);
#944=FACE_OUTER_BOUND('',#1352,.T.);
#945=FACE_OUTER_BOUND('',#1353,.T.);
#946=FACE_OUTER_BOUND('',#1354,.T.);
#947=FACE_OUTER_BOUND('',#1355,.T.);
#948=FACE_OUTER_BOUND('',#1356,.T.);
#949=FACE_OUTER_BOUND('',#1357,.T.);
#950=FACE_OUTER_BOUND('',#1358,.T.);
#951=FACE_OUTER_BOUND('',#1359,.T.);
#952=FACE_OUTER_BOUND('',#1361,.T.);
#953=FACE_OUTER_BOUND('',#1363,.T.);
#954=FACE_OUTER_BOUND('',#1364,.T.);
#955=FACE_OUTER_BOUND('',#1365,.T.);
#956=FACE_OUTER_BOUND('',#1366,.T.);
#957=FACE_OUTER_BOUND('',#1367,.T.);
#958=FACE_OUTER_BOUND('',#1369,.T.);
#959=FACE_OUTER_BOUND('',#1371,.T.);
#960=FACE_OUTER_BOUND('',#1372,.T.);
#961=FACE_OUTER_BOUND('',#1373,.T.);
#962=FACE_OUTER_BOUND('',#1375,.T.);
#963=FACE_OUTER_BOUND('',#1377,.T.);
#964=FACE_OUTER_BOUND('',#1379,.T.);
#965=FACE_OUTER_BOUND('',#1380,.T.);
#966=FACE_OUTER_BOUND('',#1381,.T.);
#967=FACE_OUTER_BOUND('',#1382,.T.);
#968=EDGE_LOOP('',(#3484,#3485,#3486,#3487,#3488,#3489,#3490,#3491));
#969=EDGE_LOOP('',(#3492));
#970=EDGE_LOOP('',(#3493,#3494,#3495,#3496,#3497,#3498,#3499,#3500,#3501,
#3502,#3503));
#971=EDGE_LOOP('',(#3504,#3505,#3506,#3507));
#972=EDGE_LOOP('',(#3508,#3509,#3510,#3511));
#973=EDGE_LOOP('',(#3512,#3513,#3514,#3515));
#974=EDGE_LOOP('',(#3516,#3517,#3518,#3519));
#975=EDGE_LOOP('',(#3520,#3521,#3522,#3523,#3524,#3525));
#976=EDGE_LOOP('',(#3526,#3527,#3528,#3529,#3530,#3531,#3532,#3533));
#977=EDGE_LOOP('',(#3534,#3535,#3536,#3537));
#978=EDGE_LOOP('',(#3538,#3539,#3540,#3541));
#979=EDGE_LOOP('',(#3542,#3543,#3544,#3545));
#980=EDGE_LOOP('',(#3546));
#981=EDGE_LOOP('',(#3547));
#982=EDGE_LOOP('',(#3548,#3549,#3550,#3551));
#983=EDGE_LOOP('',(#3552,#3553,#3554,#3555));
#984=EDGE_LOOP('',(#3556,#3557,#3558,#3559));
#985=EDGE_LOOP('',(#3560,#3561,#3562,#3563));
#986=EDGE_LOOP('',(#3564,#3565,#3566,#3567));
#987=EDGE_LOOP('',(#3568));
#988=EDGE_LOOP('',(#3569,#3570,#3571,#3572));
#989=EDGE_LOOP('',(#3573));
#990=EDGE_LOOP('',(#3574,#3575,#3576,#3577));
#991=EDGE_LOOP('',(#3578,#3579,#3580,#3581));
#992=EDGE_LOOP('',(#3582,#3583,#3584,#3585));
#993=EDGE_LOOP('',(#3586,#3587,#3588,#3589));
#994=EDGE_LOOP('',(#3590,#3591,#3592,#3593));
#995=EDGE_LOOP('',(#3594));
#996=EDGE_LOOP('',(#3595,#3596,#3597,#3598));
#997=EDGE_LOOP('',(#3599,#3600,#3601,#3602));
#998=EDGE_LOOP('',(#3603,#3604,#3605,#3606));
#999=EDGE_LOOP('',(#3607,#3608,#3609,#3610));
#1000=EDGE_LOOP('',(#3611));
#1001=EDGE_LOOP('',(#3612,#3613,#3614,#3615));
#1002=EDGE_LOOP('',(#3616));
#1003=EDGE_LOOP('',(#3617,#3618,#3619,#3620));
#1004=EDGE_LOOP('',(#3621,#3622,#3623,#3624));
#1005=EDGE_LOOP('',(#3625,#3626,#3627,#3628));
#1006=EDGE_LOOP('',(#3629,#3630,#3631,#3632));
#1007=EDGE_LOOP('',(#3633));
#1008=EDGE_LOOP('',(#3634,#3635,#3636,#3637));
#1009=EDGE_LOOP('',(#3638,#3639,#3640,#3641));
#1010=EDGE_LOOP('',(#3642,#3643,#3644,#3645));
#1011=EDGE_LOOP('',(#3646,#3647,#3648,#3649));
#1012=EDGE_LOOP('',(#3650));
#1013=EDGE_LOOP('',(#3651));
#1014=EDGE_LOOP('',(#3652,#3653,#3654,#3655));
#1015=EDGE_LOOP('',(#3656,#3657));
#1016=EDGE_LOOP('',(#3658,#3659,#3660,#3661,#3662,#3663));
#1017=EDGE_LOOP('',(#3664));
#1018=EDGE_LOOP('',(#3665));
#1019=EDGE_LOOP('',(#3666,#3667,#3668,#3669));
#1020=EDGE_LOOP('',(#3670,#3671,#3672,#3673));
#1021=EDGE_LOOP('',(#3674,#3675,#3676,#3677,#3678,#3679,#3680,#3681));
#1022=EDGE_LOOP('',(#3682,#3683,#3684,#3685));
#1023=EDGE_LOOP('',(#3686));
#1024=EDGE_LOOP('',(#3687,#3688,#3689,#3690));
#1025=EDGE_LOOP('',(#3691,#3692,#3693,#3694));
#1026=EDGE_LOOP('',(#3695,#3696,#3697,#3698));
#1027=EDGE_LOOP('',(#3699));
#1028=EDGE_LOOP('',(#3700,#3701,#3702,#3703));
#1029=EDGE_LOOP('',(#3704,#3705,#3706,#3707));
#1030=EDGE_LOOP('',(#3708));
#1031=EDGE_LOOP('',(#3709,#3710,#3711,#3712));
#1032=EDGE_LOOP('',(#3713,#3714,#3715,#3716));
#1033=EDGE_LOOP('',(#3717,#3718,#3719,#3720));
#1034=EDGE_LOOP('',(#3721));
#1035=EDGE_LOOP('',(#3722,#3723,#3724,#3725));
#1036=EDGE_LOOP('',(#3726,#3727,#3728,#3729));
#1037=EDGE_LOOP('',(#3730,#3731,#3732,#3733));
#1038=EDGE_LOOP('',(#3734));
#1039=EDGE_LOOP('',(#3735));
#1040=EDGE_LOOP('',(#3736,#3737,#3738,#3739,#3740,#3741,#3742,#3743,#3744,
#3745,#3746,#3747,#3748,#3749));
#1041=EDGE_LOOP('',(#3750,#3751,#3752,#3753,#3754,#3755,#3756,#3757,#3758,
#3759,#3760,#3761,#3762,#3763));
#1042=EDGE_LOOP('',(#3764,#3765,#3766,#3767));
#1043=EDGE_LOOP('',(#3768,#3769,#3770,#3771));
#1044=EDGE_LOOP('',(#3772,#3773,#3774,#3775));
#1045=EDGE_LOOP('',(#3776,#3777,#3778,#3779));
#1046=EDGE_LOOP('',(#3780));
#1047=EDGE_LOOP('',(#3781));
#1048=EDGE_LOOP('',(#3782,#3783,#3784,#3785));
#1049=EDGE_LOOP('',(#3786));
#1050=EDGE_LOOP('',(#3787));
#1051=EDGE_LOOP('',(#3788,#3789,#3790,#3791));
#1052=EDGE_LOOP('',(#3792,#3793,#3794,#3795));
#1053=EDGE_LOOP('',(#3796,#3797,#3798,#3799));
#1054=EDGE_LOOP('',(#3800,#3801,#3802,#3803));
#1055=EDGE_LOOP('',(#3804,#3805,#3806,#3807));
#1056=EDGE_LOOP('',(#3808,#3809,#3810,#3811));
#1057=EDGE_LOOP('',(#3812,#3813,#3814,#3815,#3816,#3817));
#1058=EDGE_LOOP('',(#3818,#3819,#3820,#3821,#3822,#3823));
#1059=EDGE_LOOP('',(#3824));
#1060=EDGE_LOOP('',(#3825));
#1061=EDGE_LOOP('',(#3826,#3827,#3828,#3829));
#1062=EDGE_LOOP('',(#3830,#3831,#3832,#3833));
#1063=EDGE_LOOP('',(#3834,#3835,#3836,#3837));
#1064=EDGE_LOOP('',(#3838));
#1065=EDGE_LOOP('',(#3839));
#1066=EDGE_LOOP('',(#3840,#3841,#3842,#3843));
#1067=EDGE_LOOP('',(#3844,#3845,#3846,#3847));
#1068=EDGE_LOOP('',(#3848,#3849,#3850,#3851));
#1069=EDGE_LOOP('',(#3852,#3853,#3854,#3855));
#1070=EDGE_LOOP('',(#3856,#3857,#3858,#3859));
#1071=EDGE_LOOP('',(#3860,#3861,#3862,#3863));
#1072=EDGE_LOOP('',(#3864,#3865,#3866,#3867));
#1073=EDGE_LOOP('',(#3868,#3869,#3870,#3871));
#1074=EDGE_LOOP('',(#3872,#3873,#3874,#3875));
#1075=EDGE_LOOP('',(#3876,#3877,#3878,#3879));
#1076=EDGE_LOOP('',(#3880,#3881,#3882,#3883));
#1077=EDGE_LOOP('',(#3884,#3885,#3886,#3887));
#1078=EDGE_LOOP('',(#3888,#3889,#3890,#3891));
#1079=EDGE_LOOP('',(#3892,#3893,#3894,#3895));
#1080=EDGE_LOOP('',(#3896,#3897,#3898,#3899));
#1081=EDGE_LOOP('',(#3900,#3901,#3902,#3903));
#1082=EDGE_LOOP('',(#3904,#3905,#3906,#3907));
#1083=EDGE_LOOP('',(#3908,#3909,#3910,#3911));
#1084=EDGE_LOOP('',(#3912,#3913,#3914,#3915));
#1085=EDGE_LOOP('',(#3916,#3917,#3918,#3919));
#1086=EDGE_LOOP('',(#3920,#3921,#3922,#3923));
#1087=EDGE_LOOP('',(#3924,#3925,#3926,#3927));
#1088=EDGE_LOOP('',(#3928,#3929,#3930,#3931));
#1089=EDGE_LOOP('',(#3932,#3933,#3934,#3935));
#1090=EDGE_LOOP('',(#3936,#3937,#3938,#3939));
#1091=EDGE_LOOP('',(#3940,#3941,#3942,#3943));
#1092=EDGE_LOOP('',(#3944,#3945,#3946,#3947));
#1093=EDGE_LOOP('',(#3948,#3949,#3950,#3951));
#1094=EDGE_LOOP('',(#3952,#3953,#3954,#3955));
#1095=EDGE_LOOP('',(#3956,#3957,#3958,#3959));
#1096=EDGE_LOOP('',(#3960,#3961,#3962,#3963));
#1097=EDGE_LOOP('',(#3964,#3965,#3966,#3967));
#1098=EDGE_LOOP('',(#3968));
#1099=EDGE_LOOP('',(#3969));
#1100=EDGE_LOOP('',(#3970));
#1101=EDGE_LOOP('',(#3971));
#1102=EDGE_LOOP('',(#3972));
#1103=EDGE_LOOP('',(#3973));
#1104=EDGE_LOOP('',(#3974));
#1105=EDGE_LOOP('',(#3975));
#1106=EDGE_LOOP('',(#3976));
#1107=EDGE_LOOP('',(#3977));
#1108=EDGE_LOOP('',(#3978));
#1109=EDGE_LOOP('',(#3979));
#1110=EDGE_LOOP('',(#3980));
#1111=EDGE_LOOP('',(#3981));
#1112=EDGE_LOOP('',(#3982));
#1113=EDGE_LOOP('',(#3983));
#1114=EDGE_LOOP('',(#3984));
#1115=EDGE_LOOP('',(#3985));
#1116=EDGE_LOOP('',(#3986));
#1117=EDGE_LOOP('',(#3987));
#1118=EDGE_LOOP('',(#3988));
#1119=EDGE_LOOP('',(#3989));
#1120=EDGE_LOOP('',(#3990));
#1121=EDGE_LOOP('',(#3991));
#1122=EDGE_LOOP('',(#3992));
#1123=EDGE_LOOP('',(#3993));
#1124=EDGE_LOOP('',(#3994));
#1125=EDGE_LOOP('',(#3995));
#1126=EDGE_LOOP('',(#3996,#3997,#3998,#3999));
#1127=EDGE_LOOP('',(#4000,#4001,#4002,#4003));
#1128=EDGE_LOOP('',(#4004));
#1129=EDGE_LOOP('',(#4005));
#1130=EDGE_LOOP('',(#4006));
#1131=EDGE_LOOP('',(#4007));
#1132=EDGE_LOOP('',(#4008));
#1133=EDGE_LOOP('',(#4009));
#1134=EDGE_LOOP('',(#4010));
#1135=EDGE_LOOP('',(#4011));
#1136=EDGE_LOOP('',(#4012));
#1137=EDGE_LOOP('',(#4013));
#1138=EDGE_LOOP('',(#4014));
#1139=EDGE_LOOP('',(#4015));
#1140=EDGE_LOOP('',(#4016));
#1141=EDGE_LOOP('',(#4017));
#1142=EDGE_LOOP('',(#4018));
#1143=EDGE_LOOP('',(#4019));
#1144=EDGE_LOOP('',(#4020));
#1145=EDGE_LOOP('',(#4021));
#1146=EDGE_LOOP('',(#4022));
#1147=EDGE_LOOP('',(#4023));
#1148=EDGE_LOOP('',(#4024));
#1149=EDGE_LOOP('',(#4025));
#1150=EDGE_LOOP('',(#4026));
#1151=EDGE_LOOP('',(#4027));
#1152=EDGE_LOOP('',(#4028));
#1153=EDGE_LOOP('',(#4029));
#1154=EDGE_LOOP('',(#4030));
#1155=EDGE_LOOP('',(#4031));
#1156=EDGE_LOOP('',(#4032,#4033,#4034,#4035));
#1157=EDGE_LOOP('',(#4036,#4037,#4038,#4039));
#1158=EDGE_LOOP('',(#4040,#4041,#4042,#4043));
#1159=EDGE_LOOP('',(#4044,#4045,#4046,#4047));
#1160=EDGE_LOOP('',(#4048,#4049,#4050,#4051));
#1161=EDGE_LOOP('',(#4052,#4053,#4054,#4055));
#1162=EDGE_LOOP('',(#4056));
#1163=EDGE_LOOP('',(#4057));
#1164=EDGE_LOOP('',(#4058,#4059,#4060,#4061));
#1165=EDGE_LOOP('',(#4062,#4063,#4064,#4065));
#1166=EDGE_LOOP('',(#4066));
#1167=EDGE_LOOP('',(#4067));
#1168=EDGE_LOOP('',(#4068,#4069,#4070,#4071));
#1169=EDGE_LOOP('',(#4072,#4073,#4074,#4075));
#1170=EDGE_LOOP('',(#4076,#4077,#4078,#4079));
#1171=EDGE_LOOP('',(#4080,#4081,#4082,#4083));
#1172=EDGE_LOOP('',(#4084));
#1173=EDGE_LOOP('',(#4085,#4086,#4087,#4088,#4089,#4090,#4091,#4092,#4093));
#1174=EDGE_LOOP('',(#4094,#4095,#4096,#4097));
#1175=EDGE_LOOP('',(#4098,#4099,#4100,#4101));
#1176=EDGE_LOOP('',(#4102,#4103,#4104,#4105));
#1177=EDGE_LOOP('',(#4106,#4107,#4108,#4109));
#1178=EDGE_LOOP('',(#4110,#4111,#4112,#4113));
#1179=EDGE_LOOP('',(#4114,#4115,#4116,#4117));
#1180=EDGE_LOOP('',(#4118));
#1181=EDGE_LOOP('',(#4119,#4120,#4121,#4122,#4123,#4124));
#1182=EDGE_LOOP('',(#4125));
#1183=EDGE_LOOP('',(#4126,#4127,#4128,#4129,#4130,#4131,#4132,#4133,#4134));
#1184=EDGE_LOOP('',(#4135,#4136,#4137,#4138,#4139,#4140,#4141,#4142,#4143));
#1185=EDGE_LOOP('',(#4144,#4145,#4146,#4147));
#1186=EDGE_LOOP('',(#4148,#4149,#4150,#4151));
#1187=EDGE_LOOP('',(#4152,#4153,#4154,#4155));
#1188=EDGE_LOOP('',(#4156,#4157,#4158,#4159));
#1189=EDGE_LOOP('',(#4160,#4161,#4162,#4163));
#1190=EDGE_LOOP('',(#4164,#4165,#4166,#4167));
#1191=EDGE_LOOP('',(#4168,#4169,#4170,#4171));
#1192=EDGE_LOOP('',(#4172));
#1193=EDGE_LOOP('',(#4173));
#1194=EDGE_LOOP('',(#4174));
#1195=EDGE_LOOP('',(#4175));
#1196=EDGE_LOOP('',(#4176,#4177,#4178,#4179));
#1197=EDGE_LOOP('',(#4180));
#1198=EDGE_LOOP('',(#4181,#4182,#4183,#4184));
#1199=EDGE_LOOP('',(#4185));
#1200=EDGE_LOOP('',(#4186));
#1201=EDGE_LOOP('',(#4187));
#1202=EDGE_LOOP('',(#4188));
#1203=EDGE_LOOP('',(#4189,#4190,#4191,#4192));
#1204=EDGE_LOOP('',(#4193,#4194,#4195,#4196));
#1205=EDGE_LOOP('',(#4197));
#1206=EDGE_LOOP('',(#4198,#4199));
#1207=EDGE_LOOP('',(#4200,#4201,#4202,#4203,#4204,#4205));
#1208=EDGE_LOOP('',(#4206,#4207,#4208,#4209,#4210,#4211,#4212,#4213,#4214,
#4215,#4216,#4217));
#1209=EDGE_LOOP('',(#4218,#4219,#4220,#4221));
#1210=EDGE_LOOP('',(#4222,#4223,#4224,#4225,#4226,#4227));
#1211=EDGE_LOOP('',(#4228,#4229,#4230));
#1212=EDGE_LOOP('',(#4231,#4232,#4233,#4234));
#1213=EDGE_LOOP('',(#4235));
#1214=EDGE_LOOP('',(#4236,#4237,#4238,#4239));
#1215=EDGE_LOOP('',(#4240,#4241,#4242,#4243));
#1216=EDGE_LOOP('',(#4244,#4245,#4246,#4247));
#1217=EDGE_LOOP('',(#4248,#4249,#4250,#4251));
#1218=EDGE_LOOP('',(#4252,#4253,#4254,#4255));
#1219=EDGE_LOOP('',(#4256,#4257,#4258,#4259));
#1220=EDGE_LOOP('',(#4260,#4261,#4262,#4263));
#1221=EDGE_LOOP('',(#4264,#4265,#4266,#4267,#4268,#4269));
#1222=EDGE_LOOP('',(#4270,#4271,#4272,#4273,#4274,#4275));
#1223=EDGE_LOOP('',(#4276));
#1224=EDGE_LOOP('',(#4277));
#1225=EDGE_LOOP('',(#4278,#4279,#4280,#4281));
#1226=EDGE_LOOP('',(#4282,#4283,#4284,#4285));
#1227=EDGE_LOOP('',(#4286,#4287,#4288,#4289));
#1228=EDGE_LOOP('',(#4290));
#1229=EDGE_LOOP('',(#4291));
#1230=EDGE_LOOP('',(#4292,#4293,#4294,#4295));
#1231=EDGE_LOOP('',(#4296,#4297,#4298,#4299));
#1232=EDGE_LOOP('',(#4300,#4301,#4302,#4303));
#1233=EDGE_LOOP('',(#4304,#4305,#4306,#4307));
#1234=EDGE_LOOP('',(#4308,#4309,#4310,#4311));
#1235=EDGE_LOOP('',(#4312,#4313,#4314,#4315));
#1236=EDGE_LOOP('',(#4316));
#1237=EDGE_LOOP('',(#4317,#4318,#4319,#4320));
#1238=EDGE_LOOP('',(#4321,#4322,#4323,#4324));
#1239=EDGE_LOOP('',(#4325));
#1240=EDGE_LOOP('',(#4326,#4327,#4328,#4329));
#1241=EDGE_LOOP('',(#4330,#4331,#4332,#4333));
#1242=EDGE_LOOP('',(#4334,#4335,#4336,#4337));
#1243=EDGE_LOOP('',(#4338,#4339,#4340,#4341));
#1244=EDGE_LOOP('',(#4342,#4343,#4344,#4345));
#1245=EDGE_LOOP('',(#4346));
#1246=EDGE_LOOP('',(#4347,#4348,#4349,#4350));
#1247=EDGE_LOOP('',(#4351,#4352,#4353,#4354));
#1248=EDGE_LOOP('',(#4355));
#1249=EDGE_LOOP('',(#4356,#4357,#4358,#4359));
#1250=EDGE_LOOP('',(#4360,#4361,#4362,#4363));
#1251=EDGE_LOOP('',(#4364,#4365,#4366,#4367));
#1252=EDGE_LOOP('',(#4368,#4369,#4370,#4371));
#1253=EDGE_LOOP('',(#4372,#4373,#4374,#4375));
#1254=EDGE_LOOP('',(#4376,#4377,#4378,#4379));
#1255=EDGE_LOOP('',(#4380,#4381,#4382,#4383));
#1256=EDGE_LOOP('',(#4384));
#1257=EDGE_LOOP('',(#4385));
#1258=EDGE_LOOP('',(#4386));
#1259=EDGE_LOOP('',(#4387));
#1260=EDGE_LOOP('',(#4388,#4389,#4390,#4391,#4392,#4393,#4394,#4395));
#1261=EDGE_LOOP('',(#4396,#4397,#4398,#4399));
#1262=EDGE_LOOP('',(#4400));
#1263=EDGE_LOOP('',(#4401,#4402,#4403,#4404));
#1264=EDGE_LOOP('',(#4405,#4406,#4407,#4408));
#1265=EDGE_LOOP('',(#4409,#4410,#4411,#4412));
#1266=EDGE_LOOP('',(#4413,#4414,#4415,#4416,#4417,#4418,#4419,#4420));
#1267=EDGE_LOOP('',(#4421,#4422,#4423,#4424));
#1268=EDGE_LOOP('',(#4425));
#1269=EDGE_LOOP('',(#4426,#4427,#4428,#4429));
#1270=EDGE_LOOP('',(#4430));
#1271=EDGE_LOOP('',(#4431,#4432,#4433,#4434));
#1272=EDGE_LOOP('',(#4435));
#1273=EDGE_LOOP('',(#4436));
#1274=EDGE_LOOP('',(#4437));
#1275=EDGE_LOOP('',(#4438,#4439,#4440,#4441));
#1276=EDGE_LOOP('',(#4442,#4443,#4444,#4445));
#1277=EDGE_LOOP('',(#4446,#4447,#4448,#4449));
#1278=EDGE_LOOP('',(#4450,#4451,#4452,#4453));
#1279=EDGE_LOOP('',(#4454,#4455,#4456,#4457));
#1280=EDGE_LOOP('',(#4458,#4459,#4460,#4461));
#1281=EDGE_LOOP('',(#4462,#4463,#4464,#4465,#4466,#4467));
#1282=EDGE_LOOP('',(#4468,#4469,#4470,#4471,#4472,#4473));
#1283=EDGE_LOOP('',(#4474));
#1284=EDGE_LOOP('',(#4475));
#1285=EDGE_LOOP('',(#4476,#4477,#4478,#4479));
#1286=EDGE_LOOP('',(#4480,#4481,#4482,#4483));
#1287=EDGE_LOOP('',(#4484,#4485,#4486,#4487));
#1288=EDGE_LOOP('',(#4488));
#1289=EDGE_LOOP('',(#4489));
#1290=EDGE_LOOP('',(#4490,#4491,#4492,#4493));
#1291=EDGE_LOOP('',(#4494,#4495,#4496,#4497));
#1292=EDGE_LOOP('',(#4498,#4499,#4500,#4501));
#1293=EDGE_LOOP('',(#4502,#4503,#4504,#4505));
#1294=EDGE_LOOP('',(#4506,#4507,#4508,#4509));
#1295=EDGE_LOOP('',(#4510,#4511,#4512,#4513));
#1296=EDGE_LOOP('',(#4514,#4515,#4516,#4517));
#1297=EDGE_LOOP('',(#4518));
#1298=EDGE_LOOP('',(#4519));
#1299=EDGE_LOOP('',(#4520,#4521,#4522,#4523));
#1300=EDGE_LOOP('',(#4524,#4525,#4526,#4527));
#1301=EDGE_LOOP('',(#4528,#4529,#4530,#4531));
#1302=EDGE_LOOP('',(#4532));
#1303=EDGE_LOOP('',(#4533));
#1304=EDGE_LOOP('',(#4534,#4535,#4536,#4537));
#1305=EDGE_LOOP('',(#4538));
#1306=EDGE_LOOP('',(#4539,#4540,#4541,#4542));
#1307=EDGE_LOOP('',(#4543,#4544,#4545,#4546));
#1308=EDGE_LOOP('',(#4547,#4548,#4549,#4550));
#1309=EDGE_LOOP('',(#4551,#4552,#4553,#4554));
#1310=EDGE_LOOP('',(#4555));
#1311=EDGE_LOOP('',(#4556,#4557,#4558,#4559,#4560,#4561,#4562,#4563));
#1312=EDGE_LOOP('',(#4564,#4565,#4566,#4567));
#1313=EDGE_LOOP('',(#4568));
#1314=EDGE_LOOP('',(#4569,#4570,#4571,#4572));
#1315=EDGE_LOOP('',(#4573,#4574,#4575,#4576));
#1316=EDGE_LOOP('',(#4577));
#1317=EDGE_LOOP('',(#4578,#4579,#4580,#4581,#4582,#4583,#4584,#4585));
#1318=EDGE_LOOP('',(#4586,#4587,#4588,#4589));
#1319=EDGE_LOOP('',(#4590));
#1320=EDGE_LOOP('',(#4591,#4592,#4593,#4594));
#1321=EDGE_LOOP('',(#4595,#4596,#4597,#4598));
#1322=EDGE_LOOP('',(#4599));
#1323=EDGE_LOOP('',(#4600,#4601,#4602,#4603));
#1324=EDGE_LOOP('',(#4604));
#1325=EDGE_LOOP('',(#4605));
#1326=EDGE_LOOP('',(#4606,#4607,#4608,#4609));
#1327=EDGE_LOOP('',(#4610,#4611,#4612,#4613));
#1328=EDGE_LOOP('',(#4614));
#1329=EDGE_LOOP('',(#4615,#4616,#4617,#4618,#4619,#4620,#4621,#4622,#4623));
#1330=EDGE_LOOP('',(#4624,#4625,#4626,#4627));
#1331=EDGE_LOOP('',(#4628,#4629,#4630,#4631));
#1332=EDGE_LOOP('',(#4632,#4633,#4634,#4635));
#1333=EDGE_LOOP('',(#4636,#4637,#4638,#4639));
#1334=EDGE_LOOP('',(#4640,#4641,#4642,#4643));
#1335=EDGE_LOOP('',(#4644,#4645,#4646,#4647));
#1336=EDGE_LOOP('',(#4648));
#1337=EDGE_LOOP('',(#4649,#4650,#4651,#4652,#4653,#4654));
#1338=EDGE_LOOP('',(#4655));
#1339=EDGE_LOOP('',(#4656,#4657,#4658,#4659,#4660,#4661,#4662,#4663,#4664));
#1340=EDGE_LOOP('',(#4665,#4666,#4667,#4668,#4669,#4670,#4671,#4672,#4673));
#1341=EDGE_LOOP('',(#4674,#4675,#4676,#4677));
#1342=EDGE_LOOP('',(#4678,#4679,#4680,#4681));
#1343=EDGE_LOOP('',(#4682,#4683,#4684,#4685));
#1344=EDGE_LOOP('',(#4686,#4687,#4688,#4689));
#1345=EDGE_LOOP('',(#4690,#4691,#4692,#4693));
#1346=EDGE_LOOP('',(#4694,#4695,#4696,#4697));
#1347=EDGE_LOOP('',(#4698,#4699,#4700,#4701));
#1348=EDGE_LOOP('',(#4702));
#1349=EDGE_LOOP('',(#4703));
#1350=EDGE_LOOP('',(#4704));
#1351=EDGE_LOOP('',(#4705));
#1352=EDGE_LOOP('',(#4706,#4707,#4708,#4709));
#1353=EDGE_LOOP('',(#4710));
#1354=EDGE_LOOP('',(#4711));
#1355=EDGE_LOOP('',(#4712,#4713,#4714,#4715,#4716,#4717));
#1356=EDGE_LOOP('',(#4718));
#1357=EDGE_LOOP('',(#4719,#4720,#4721,#4722));
#1358=EDGE_LOOP('',(#4723,#4724,#4725,#4726));
#1359=EDGE_LOOP('',(#4727));
#1360=EDGE_LOOP('',(#4728));
#1361=EDGE_LOOP('',(#4729,#4730,#4731,#4732,#4733,#4734,#4735,#4736,#4737));
#1362=EDGE_LOOP('',(#4738));
#1363=EDGE_LOOP('',(#4739,#4740,#4741,#4742));
#1364=EDGE_LOOP('',(#4743));
#1365=EDGE_LOOP('',(#4744,#4745,#4746,#4747));
#1366=EDGE_LOOP('',(#4748,#4749,#4750,#4751));
#1367=EDGE_LOOP('',(#4752));
#1368=EDGE_LOOP('',(#4753));
#1369=EDGE_LOOP('',(#4754));
#1370=EDGE_LOOP('',(#4755));
#1371=EDGE_LOOP('',(#4756,#4757,#4758,#4759));
#1372=EDGE_LOOP('',(#4760,#4761,#4762,#4763));
#1373=EDGE_LOOP('',(#4764));
#1374=EDGE_LOOP('',(#4765));
#1375=EDGE_LOOP('',(#4766));
#1376=EDGE_LOOP('',(#4767));
#1377=EDGE_LOOP('',(#4768,#4769,#4770,#4771));
#1378=EDGE_LOOP('',(#4772,#4773));
#1379=EDGE_LOOP('',(#4774,#4775));
#1380=EDGE_LOOP('',(#4776,#4777,#4778,#4779));
#1381=EDGE_LOOP('',(#4780,#4781,#4782,#4783,#4784,#4785,#4786,#4787,#4788));
#1382=EDGE_LOOP('',(#4789,#4790,#4791));
#1383=CIRCLE('',#5465,0.3);
#1384=CIRCLE('',#5466,0.3);
#1385=CIRCLE('',#5467,0.3);
#1386=CIRCLE('',#5468,0.3);
#1387=CIRCLE('',#5477,0.275);
#1388=CIRCLE('',#5478,0.275);
#1389=CIRCLE('',#5480,0.275);
#1390=CIRCLE('',#5482,0.275);
#1391=CIRCLE('',#5484,0.51);
#1392=CIRCLE('',#5485,0.51);
#1393=CIRCLE('',#5492,0.31);
#1394=CIRCLE('',#5493,0.31);
#1395=CIRCLE('',#5495,0.31);
#1396=CIRCLE('',#5496,0.31);
#1397=CIRCLE('',#5513,0.6);
#1398=CIRCLE('',#5514,0.6);
#1399=CIRCLE('',#5517,0.33);
#1400=CIRCLE('',#5518,0.33);
#1401=CIRCLE('',#5520,0.33);
#1402=CIRCLE('',#5522,0.33);
#1403=CIRCLE('',#5525,0.210000000000001);
#1404=CIRCLE('',#5526,0.210000000000001);
#1405=CIRCLE('',#5533,0.21);
#1406=CIRCLE('',#5534,0.21);
#1407=CIRCLE('',#5548,0.285);
#1408=CIRCLE('',#5549,0.265);
#1409=CIRCLE('',#5551,0.265);
#1410=CIRCLE('',#5553,0.5);
#1411=CIRCLE('',#5555,0.5);
#1412=CIRCLE('',#5567,0.24505);
#1413=CIRCLE('',#5569,0.375);
#1414=CIRCLE('',#5571,0.425);
#1415=CIRCLE('',#5573,0.425);
#1416=CIRCLE('',#5575,0.395);
#1417=CIRCLE('',#5577,0.27);
#1418=CIRCLE('',#5579,0.24505);
#1419=CIRCLE('',#5583,0.3);
#1420=CIRCLE('',#5584,0.3);
#1421=CIRCLE('',#5586,0.3);
#1422=CIRCLE('',#5587,0.3);
#1423=CIRCLE('',#5589,0.33);
#1424=CIRCLE('',#5590,0.33);
#1425=CIRCLE('',#5592,0.33);
#1426=CIRCLE('',#5593,0.33);
#1427=CIRCLE('',#5595,0.33);
#1428=CIRCLE('',#5596,0.33);
#1429=CIRCLE('',#5598,0.33);
#1430=CIRCLE('',#5599,0.33);
#1431=CIRCLE('',#5601,0.33);
#1432=CIRCLE('',#5602,0.33);
#1433=CIRCLE('',#5604,0.33);
#1434=CIRCLE('',#5605,0.33);
#1435=CIRCLE('',#5607,0.34);
#1436=CIRCLE('',#5608,0.34);
#1437=CIRCLE('',#5610,0.34);
#1438=CIRCLE('',#5611,0.34);
#1439=CIRCLE('',#5613,0.34);
#1440=CIRCLE('',#5614,0.34);
#1441=CIRCLE('',#5616,0.34);
#1442=CIRCLE('',#5617,0.34);
#1443=CIRCLE('',#5619,0.34);
#1444=CIRCLE('',#5620,0.34);
#1445=CIRCLE('',#5622,0.34);
#1446=CIRCLE('',#5623,0.34);
#1447=CIRCLE('',#5625,0.34);
#1448=CIRCLE('',#5626,0.34);
#1449=CIRCLE('',#5628,0.34);
#1450=CIRCLE('',#5629,0.34);
#1451=CIRCLE('',#5631,0.34);
#1452=CIRCLE('',#5632,0.34);
#1453=CIRCLE('',#5634,0.34);
#1454=CIRCLE('',#5635,0.34);
#1455=CIRCLE('',#5637,0.34);
#1456=CIRCLE('',#5638,0.34);
#1457=CIRCLE('',#5640,0.34);
#1458=CIRCLE('',#5641,0.34);
#1459=CIRCLE('',#5643,0.34);
#1460=CIRCLE('',#5644,0.34);
#1461=CIRCLE('',#5646,0.34);
#1462=CIRCLE('',#5647,0.34);
#1463=CIRCLE('',#5649,0.34);
#1464=CIRCLE('',#5650,0.34);
#1465=CIRCLE('',#5652,0.34);
#1466=CIRCLE('',#5653,0.34);
#1467=CIRCLE('',#5655,0.34);
#1468=CIRCLE('',#5656,0.34);
#1469=CIRCLE('',#5658,0.34);
#1470=CIRCLE('',#5659,0.34);
#1471=CIRCLE('',#5661,0.34);
#1472=CIRCLE('',#5662,0.34);
#1473=CIRCLE('',#5664,0.34);
#1474=CIRCLE('',#5665,0.34);
#1475=CIRCLE('',#5674,0.425);
#1476=CIRCLE('',#5675,0.425);
#1477=CIRCLE('',#5677,0.425);
#1478=CIRCLE('',#5678,0.425);
#1479=CIRCLE('',#5687,0.2942);
#1480=CIRCLE('',#5688,0.2942);
#1481=CIRCLE('',#5690,0.24);
#1482=CIRCLE('',#5693,0.475);
#1483=CIRCLE('',#5704,0.475);
#1484=CIRCLE('',#5706,0.475);
#1485=CIRCLE('',#5711,0.25175);
#1486=CIRCLE('',#5712,0.25175);
#1487=CIRCLE('',#5720,0.4);
#1488=CIRCLE('',#5721,0.4);
#1489=CIRCLE('',#5724,0.8);
#1490=CIRCLE('',#5725,0.8);
#1491=CIRCLE('',#5730,0.3);
#1492=CIRCLE('',#5732,0.3);
#1493=CIRCLE('',#5734,0.22);
#1494=CIRCLE('',#5738,0.3);
#1495=CIRCLE('',#5741,0.3);
#1496=CIRCLE('',#5742,0.3);
#1497=CIRCLE('',#5743,0.3);
#1498=CIRCLE('',#5744,0.3);
#1499=CIRCLE('',#5745,0.3);
#1500=CIRCLE('',#5747,0.22);
#1501=CIRCLE('',#5751,0.22);
#1502=CIRCLE('',#5764,0.3933);
#1503=CIRCLE('',#5766,0.6);
#1504=CIRCLE('',#5768,0.65);
#1505=CIRCLE('',#5770,0.65);
#1506=CIRCLE('',#5772,0.62);
#1507=CIRCLE('',#5774,0.42);
#1508=CIRCLE('',#5776,0.3933);
#1509=CIRCLE('',#5781,0.275);
#1510=CIRCLE('',#5782,0.275);
#1511=CIRCLE('',#5784,0.31);
#1512=CIRCLE('',#5785,0.31);
#1513=CIRCLE('',#5787,0.7);
#1514=CIRCLE('',#5788,0.7);
#1515=CIRCLE('',#5790,0.6);
#1516=CIRCLE('',#5793,0.6);
#1517=CIRCLE('',#5796,0.31);
#1518=CIRCLE('',#5797,0.31);
#1519=CIRCLE('',#5799,0.31);
#1520=CIRCLE('',#5800,0.31);
#1521=CIRCLE('',#5806,0.6);
#1522=CIRCLE('',#5809,0.6);
#1523=CIRCLE('',#5812,0.6);
#1524=CIRCLE('',#5813,0.6);
#1525=CIRCLE('',#5824,0.21);
#1526=CIRCLE('',#5825,0.21);
#1527=CIRCLE('',#5828,0.7);
#1528=CIRCLE('',#5829,0.7);
#1529=CIRCLE('',#5842,0.24505);
#1530=CIRCLE('',#5844,0.375);
#1531=CIRCLE('',#5846,0.425);
#1532=CIRCLE('',#5848,0.425);
#1533=CIRCLE('',#5850,0.395);
#1534=CIRCLE('',#5852,0.27);
#1535=CIRCLE('',#5854,0.24505);
#1536=CIRCLE('',#5859,0.31);
#1537=CIRCLE('',#5860,0.31);
#1538=CIRCLE('',#5862,0.31);
#1539=CIRCLE('',#5863,0.31);
#1540=CIRCLE('',#5865,0.6);
#1541=CIRCLE('',#5866,0.6);
#1542=CIRCLE('',#5869,0.6);
#1543=CIRCLE('',#5872,0.6);
#1544=CIRCLE('',#5878,0.34);
#1545=CIRCLE('',#5879,0.34);
#1546=CIRCLE('',#5882,0.31);
#1547=CIRCLE('',#5883,0.31);
#1548=CIRCLE('',#5885,0.31);
#1549=CIRCLE('',#5886,0.31);
#1550=CIRCLE('',#5893,0.5);
#1551=CIRCLE('',#5899,0.5);
#1552=CIRCLE('',#5903,0.3933);
#1553=CIRCLE('',#5904,0.3933);
#1554=CIRCLE('',#5906,0.32);
#1555=CIRCLE('',#5909,0.6175);
#1556=CIRCLE('',#5920,0.6175);
#1557=CIRCLE('',#5922,0.6175);
#1558=CIRCLE('',#5927,0.338975);
#1559=CIRCLE('',#5928,0.338975);
#1560=CIRCLE('',#5936,1.);
#1561=CIRCLE('',#5937,1.);
#1562=CIRCLE('',#5943,0.45);
#1563=CIRCLE('',#5945,0.5);
#1564=CIRCLE('',#5947,0.5);
#1565=CIRCLE('',#5949,0.3);
#1566=CIRCLE('',#5951,0.3);
#1567=CIRCLE('',#5953,0.21);
#1568=CIRCLE('',#5957,0.32);
#1569=CIRCLE('',#5958,0.32);
#1570=CIRCLE('',#5960,0.6);
#1571=CIRCLE('',#5961,0.6);
#1572=CIRCLE('',#5966,0.31);
#1573=CIRCLE('',#5967,0.31);
#1574=CIRCLE('',#5969,0.5);
#1575=CIRCLE('',#5970,0.5);
#1576=CIRCLE('',#5975,0.08);
#1577=CIRCLE('',#5976,0.04);
#1578=CIRCLE('',#5978,0.08);
#1579=CIRCLE('',#5981,0.08);
#1580=CIRCLE('',#5982,0.08);
#1581=LINE('',#7581,#1991);
#1582=LINE('',#7585,#1992);
#1583=LINE('',#7589,#1993);
#1584=LINE('',#7595,#1994);
#1585=LINE('',#7597,#1995);
#1586=LINE('',#7599,#1996);
#1587=LINE('',#7601,#1997);
#1588=LINE('',#7603,#1998);
#1589=LINE('',#7605,#1999);
#1590=LINE('',#7607,#2000);
#1591=LINE('',#7609,#2001);
#1592=LINE('',#7610,#2002);
#1593=LINE('',#7613,#2003);
#1594=LINE('',#7614,#2004);
#1595=LINE('',#7617,#2005);
#1596=LINE('',#7618,#2006);
#1597=LINE('',#7621,#2007);
#1598=LINE('',#7622,#2008);
#1599=LINE('',#7625,#2009);
#1600=LINE('',#7626,#2010);
#1601=LINE('',#7628,#2011);
#1602=LINE('',#7631,#2012);
#1603=LINE('',#7633,#2013);
#1604=LINE('',#7634,#2014);
#1605=LINE('',#7637,#2015);
#1606=LINE('',#7639,#2016);
#1607=LINE('',#7641,#2017);
#1608=LINE('',#7642,#2018);
#1609=LINE('',#7645,#2019);
#1610=LINE('',#7647,#2020);
#1611=LINE('',#7649,#2021);
#1612=LINE('',#7650,#2022);
#1613=LINE('',#7653,#2023);
#1614=LINE('',#7655,#2024);
#1615=LINE('',#7657,#2025);
#1616=LINE('',#7658,#2026);
#1617=LINE('',#7666,#2027);
#1618=LINE('',#7670,#2028);
#1619=LINE('',#7675,#2029);
#1620=LINE('',#7679,#2030);
#1621=LINE('',#7681,#2031);
#1622=LINE('',#7682,#2032);
#1623=LINE('',#7685,#2033);
#1624=LINE('',#7686,#2034);
#1625=LINE('',#7689,#2035);
#1626=LINE('',#7690,#2036);
#1627=LINE('',#7692,#2037);
#1628=LINE('',#7698,#2038);
#1629=LINE('',#7704,#2039);
#1630=LINE('',#7708,#2040);
#1631=LINE('',#7710,#2041);
#1632=LINE('',#7711,#2042);
#1633=LINE('',#7714,#2043);
#1634=LINE('',#7715,#2044);
#1635=LINE('',#7718,#2045);
#1636=LINE('',#7719,#2046);
#1637=LINE('',#7721,#2047);
#1638=LINE('',#7725,#2048);
#1639=LINE('',#7727,#2049);
#1640=LINE('',#7728,#2050);
#1641=LINE('',#7731,#2051);
#1642=LINE('',#7732,#2052);
#1643=LINE('',#7735,#2053);
#1644=LINE('',#7736,#2054);
#1645=LINE('',#7738,#2055);
#1646=LINE('',#7742,#2056);
#1647=LINE('',#7743,#2057);
#1648=LINE('',#7746,#2058);
#1649=LINE('',#7747,#2059);
#1650=LINE('',#7749,#2060);
#1651=LINE('',#7755,#2061);
#1652=LINE('',#7759,#2062);
#1653=LINE('',#7762,#2063);
#1654=LINE('',#7765,#2064);
#1655=LINE('',#7767,#2065);
#1656=LINE('',#7769,#2066);
#1657=LINE('',#7771,#2067);
#1658=LINE('',#7772,#2068);
#1659=LINE('',#7779,#2069);
#1660=LINE('',#7783,#2070);
#1661=LINE('',#7787,#2071);
#1662=LINE('',#7789,#2072);
#1663=LINE('',#7790,#2073);
#1664=LINE('',#7795,#2074);
#1665=LINE('',#7800,#2075);
#1666=LINE('',#7802,#2076);
#1667=LINE('',#7803,#2077);
#1668=LINE('',#7807,#2078);
#1669=LINE('',#7809,#2079);
#1670=LINE('',#7811,#2080);
#1671=LINE('',#7812,#2081);
#1672=LINE('',#7814,#2082);
#1673=LINE('',#7815,#2083);
#1674=LINE('',#7818,#2084);
#1675=LINE('',#7820,#2085);
#1676=LINE('',#7821,#2086);
#1677=LINE('',#7826,#2087);
#1678=LINE('',#7831,#2088);
#1679=LINE('',#7833,#2089);
#1680=LINE('',#7834,#2090);
#1681=LINE('',#7838,#2091);
#1682=LINE('',#7840,#2092);
#1683=LINE('',#7842,#2093);
#1684=LINE('',#7843,#2094);
#1685=LINE('',#7845,#2095);
#1686=LINE('',#7846,#2096);
#1687=LINE('',#7849,#2097);
#1688=LINE('',#7851,#2098);
#1689=LINE('',#7852,#2099);
#1690=LINE('',#7855,#2100);
#1691=LINE('',#7857,#2101);
#1692=LINE('',#7858,#2102);
#1693=LINE('',#7861,#2103);
#1694=LINE('',#7863,#2104);
#1695=LINE('',#7864,#2105);
#1696=LINE('',#7867,#2106);
#1697=LINE('',#7868,#2107);
#1698=LINE('',#7871,#2108);
#1699=LINE('',#7872,#2109);
#1700=LINE('',#7874,#2110);
#1701=LINE('',#7881,#2111);
#1702=LINE('',#7885,#2112);
#1703=LINE('',#7892,#2113);
#1704=LINE('',#7899,#2114);
#1705=LINE('',#7901,#2115);
#1706=LINE('',#7903,#2116);
#1707=LINE('',#7904,#2117);
#1708=LINE('',#7907,#2118);
#1709=LINE('',#7909,#2119);
#1710=LINE('',#7910,#2120);
#1711=LINE('',#7913,#2121);
#1712=LINE('',#7915,#2122);
#1713=LINE('',#7916,#2123);
#1714=LINE('',#7919,#2124);
#1715=LINE('',#7921,#2125);
#1716=LINE('',#7922,#2126);
#1717=LINE('',#7925,#2127);
#1718=LINE('',#7927,#2128);
#1719=LINE('',#7928,#2129);
#1720=LINE('',#7930,#2130);
#1721=LINE('',#7931,#2131);
#1722=LINE('',#7943,#2132);
#1723=LINE('',#7947,#2133);
#1724=LINE('',#7951,#2134);
#1725=LINE('',#7958,#2135);
#1726=LINE('',#7960,#2136);
#1727=LINE('',#7966,#2137);
#1728=LINE('',#7972,#2138);
#1729=LINE('',#7978,#2139);
#1730=LINE('',#7984,#2140);
#1731=LINE('',#7990,#2141);
#1732=LINE('',#7996,#2142);
#1733=LINE('',#8002,#2143);
#1734=LINE('',#8008,#2144);
#1735=LINE('',#8014,#2145);
#1736=LINE('',#8020,#2146);
#1737=LINE('',#8026,#2147);
#1738=LINE('',#8032,#2148);
#1739=LINE('',#8038,#2149);
#1740=LINE('',#8044,#2150);
#1741=LINE('',#8050,#2151);
#1742=LINE('',#8056,#2152);
#1743=LINE('',#8062,#2153);
#1744=LINE('',#8068,#2154);
#1745=LINE('',#8074,#2155);
#1746=LINE('',#8080,#2156);
#1747=LINE('',#8086,#2157);
#1748=LINE('',#8092,#2158);
#1749=LINE('',#8098,#2159);
#1750=LINE('',#8104,#2160);
#1751=LINE('',#8110,#2161);
#1752=LINE('',#8116,#2162);
#1753=LINE('',#8122,#2163);
#1754=LINE('',#8128,#2164);
#1755=LINE('',#8133,#2165);
#1756=LINE('',#8135,#2166);
#1757=LINE('',#8137,#2167);
#1758=LINE('',#8138,#2168);
#1759=LINE('',#8141,#2169);
#1760=LINE('',#8143,#2170);
#1761=LINE('',#8144,#2171);
#1762=LINE('',#8147,#2172);
#1763=LINE('',#8149,#2173);
#1764=LINE('',#8150,#2174);
#1765=LINE('',#8152,#2175);
#1766=LINE('',#8153,#2176);
#1767=LINE('',#8161,#2177);
#1768=LINE('',#8167,#2178);
#1769=LINE('',#8172,#2179);
#1770=LINE('',#8174,#2180);
#1771=LINE('',#8176,#2181);
#1772=LINE('',#8177,#2182);
#1773=LINE('',#8180,#2183);
#1774=LINE('',#8182,#2184);
#1775=LINE('',#8183,#2185);
#1776=LINE('',#8186,#2186);
#1777=LINE('',#8188,#2187);
#1778=LINE('',#8189,#2188);
#1779=LINE('',#8191,#2189);
#1780=LINE('',#8192,#2190);
#1781=LINE('',#8200,#2191);
#1782=LINE('',#8205,#2192);
#1783=LINE('',#8211,#2193);
#1784=LINE('',#8237,#2194);
#1785=LINE('',#8239,#2195);
#1786=LINE('',#8240,#2196);
#1787=LINE('',#8243,#2197);
#1788=LINE('',#8244,#2198);
#1789=LINE('',#8247,#2199);
#1790=LINE('',#8248,#2200);
#1791=LINE('',#8251,#2201);
#1792=LINE('',#8252,#2202);
#1793=LINE('',#8255,#2203);
#1794=LINE('',#8256,#2204);
#1795=LINE('',#8258,#2205);
#1796=LINE('',#8273,#2206);
#1797=LINE('',#8294,#2207);
#1798=LINE('',#8319,#2208);
#1799=LINE('',#8320,#2209);
#1800=LINE('',#8322,#2210);
#1801=LINE('',#8324,#2211);
#1802=LINE('',#8329,#2212);
#1803=LINE('',#8332,#2213);
#1804=LINE('',#8334,#2214);
#1805=LINE('',#8343,#2215);
#1806=LINE('',#8350,#2216);
#1807=LINE('',#8361,#2217);
#1808=LINE('',#8365,#2218);
#1809=LINE('',#8372,#2219);
#1810=LINE('',#8375,#2220);
#1811=LINE('',#8381,#2221);
#1812=LINE('',#8386,#2222);
#1813=LINE('',#8391,#2223);
#1814=LINE('',#8395,#2224);
#1815=LINE('',#8400,#2225);
#1816=LINE('',#8409,#2226);
#1817=LINE('',#8411,#2227);
#1818=LINE('',#8424,#2228);
#1819=LINE('',#8426,#2229);
#1820=LINE('',#8428,#2230);
#1821=LINE('',#8429,#2231);
#1822=LINE('',#8432,#2232);
#1823=LINE('',#8434,#2233);
#1824=LINE('',#8435,#2234);
#1825=LINE('',#8438,#2235);
#1826=LINE('',#8440,#2236);
#1827=LINE('',#8441,#2237);
#1828=LINE('',#8444,#2238);
#1829=LINE('',#8446,#2239);
#1830=LINE('',#8447,#2240);
#1831=LINE('',#8450,#2241);
#1832=LINE('',#8452,#2242);
#1833=LINE('',#8453,#2243);
#1834=LINE('',#8455,#2244);
#1835=LINE('',#8456,#2245);
#1836=LINE('',#8468,#2246);
#1837=LINE('',#8472,#2247);
#1838=LINE('',#8476,#2248);
#1839=LINE('',#8483,#2249);
#1840=LINE('',#8485,#2250);
#1841=LINE('',#8492,#2251);
#1842=LINE('',#8498,#2252);
#1843=LINE('',#8503,#2253);
#1844=LINE('',#8507,#2254);
#1845=LINE('',#8511,#2255);
#1846=LINE('',#8514,#2256);
#1847=LINE('',#8517,#2257);
#1848=LINE('',#8518,#2258);
#1849=LINE('',#8521,#2259);
#1850=LINE('',#8524,#2260);
#1851=LINE('',#8529,#2261);
#1852=LINE('',#8535,#2262);
#1853=LINE('',#8540,#2263);
#1854=LINE('',#8542,#2264);
#1855=LINE('',#8544,#2265);
#1856=LINE('',#8545,#2266);
#1857=LINE('',#8549,#2267);
#1858=LINE('',#8551,#2268);
#1859=LINE('',#8553,#2269);
#1860=LINE('',#8554,#2270);
#1861=LINE('',#8558,#2271);
#1862=LINE('',#8559,#2272);
#1863=LINE('',#8560,#2273);
#1864=LINE('',#8562,#2274);
#1865=LINE('',#8563,#2275);
#1866=LINE('',#8567,#2276);
#1867=LINE('',#8569,#2277);
#1868=LINE('',#8572,#2278);
#1869=LINE('',#8575,#2279);
#1870=LINE('',#8577,#2280);
#1871=LINE('',#8578,#2281);
#1872=LINE('',#8581,#2282);
#1873=LINE('',#8583,#2283);
#1874=LINE('',#8586,#2284);
#1875=LINE('',#8587,#2285);
#1876=LINE('',#8592,#2286);
#1877=LINE('',#8598,#2287);
#1878=LINE('',#8600,#2288);
#1879=LINE('',#8602,#2289);
#1880=LINE('',#8603,#2290);
#1881=LINE('',#8606,#2291);
#1882=LINE('',#8607,#2292);
#1883=LINE('',#8610,#2293);
#1884=LINE('',#8611,#2294);
#1885=LINE('',#8614,#2295);
#1886=LINE('',#8615,#2296);
#1887=LINE('',#8617,#2297);
#1888=LINE('',#8624,#2298);
#1889=LINE('',#8631,#2299);
#1890=LINE('',#8639,#2300);
#1891=LINE('',#8641,#2301);
#1892=LINE('',#8643,#2302);
#1893=LINE('',#8644,#2303);
#1894=LINE('',#8647,#2304);
#1895=LINE('',#8649,#2305);
#1896=LINE('',#8650,#2306);
#1897=LINE('',#8653,#2307);
#1898=LINE('',#8655,#2308);
#1899=LINE('',#8656,#2309);
#1900=LINE('',#8659,#2310);
#1901=LINE('',#8661,#2311);
#1902=LINE('',#8662,#2312);
#1903=LINE('',#8665,#2313);
#1904=LINE('',#8667,#2314);
#1905=LINE('',#8668,#2315);
#1906=LINE('',#8670,#2316);
#1907=LINE('',#8671,#2317);
#1908=LINE('',#8683,#2318);
#1909=LINE('',#8687,#2319);
#1910=LINE('',#8691,#2320);
#1911=LINE('',#8698,#2321);
#1912=LINE('',#8700,#2322);
#1913=LINE('',#8707,#2323);
#1914=LINE('',#8713,#2324);
#1915=LINE('',#8718,#2325);
#1916=LINE('',#8722,#2326);
#1917=LINE('',#8726,#2327);
#1918=LINE('',#8728,#2328);
#1919=LINE('',#8729,#2329);
#1920=LINE('',#8732,#2330);
#1921=LINE('',#8736,#2331);
#1922=LINE('',#8737,#2332);
#1923=LINE('',#8748,#2333);
#1924=LINE('',#8755,#2334);
#1925=LINE('',#8761,#2335);
#1926=LINE('',#8766,#2336);
#1927=LINE('',#8768,#2337);
#1928=LINE('',#8770,#2338);
#1929=LINE('',#8771,#2339);
#1930=LINE('',#8775,#2340);
#1931=LINE('',#8777,#2341);
#1932=LINE('',#8779,#2342);
#1933=LINE('',#8780,#2343);
#1934=LINE('',#8783,#2344);
#1935=LINE('',#8784,#2345);
#1936=LINE('',#8786,#2346);
#1937=LINE('',#8788,#2347);
#1938=LINE('',#8790,#2348);
#1939=LINE('',#8791,#2349);
#1940=LINE('',#8795,#2350);
#1941=LINE('',#8796,#2351);
#1942=LINE('',#8797,#2352);
#1943=LINE('',#8800,#2353);
#1944=LINE('',#8801,#2354);
#1945=LINE('',#8803,#2355);
#1946=LINE('',#8807,#2356);
#1947=LINE('',#8809,#2357);
#1948=LINE('',#8810,#2358);
#1949=LINE('',#8813,#2359);
#1950=LINE('',#8818,#2360);
#1951=LINE('',#8825,#2361);
#1952=LINE('',#8830,#2362);
#1953=LINE('',#8836,#2363);
#1954=LINE('',#8862,#2364);
#1955=LINE('',#8864,#2365);
#1956=LINE('',#8865,#2366);
#1957=LINE('',#8868,#2367);
#1958=LINE('',#8869,#2368);
#1959=LINE('',#8872,#2369);
#1960=LINE('',#8873,#2370);
#1961=LINE('',#8876,#2371);
#1962=LINE('',#8877,#2372);
#1963=LINE('',#8880,#2373);
#1964=LINE('',#8881,#2374);
#1965=LINE('',#8883,#2375);
#1966=LINE('',#8898,#2376);
#1967=LINE('',#8919,#2377);
#1968=LINE('',#8944,#2378);
#1969=LINE('',#8945,#2379);
#1970=LINE('',#8947,#2380);
#1971=LINE('',#8949,#2381);
#1972=LINE('',#8954,#2382);
#1973=LINE('',#8957,#2383);
#1974=LINE('',#8959,#2384);
#1975=LINE('',#8968,#2385);
#1976=LINE('',#8987,#2386);
#1977=LINE('',#9057,#2387);
#1978=LINE('',#9061,#2388);
#1979=LINE('',#9068,#2389);
#1980=LINE('',#9069,#2390);
#1981=LINE('',#9073,#2391);
#1982=LINE('',#9080,#2392);
#1983=LINE('',#9086,#2393);
#1984=LINE('',#9095,#2394);
#1985=LINE('',#9101,#2395);
#1986=LINE('',#9168,#2396);
#1987=LINE('',#9171,#2397);
#1988=LINE('',#9173,#2398);
#1989=LINE('',#9174,#2399);
#1990=LINE('',#9178,#2400);
#1991=VECTOR('',#6037,1.);
#1992=VECTOR('',#6040,1.);
#1993=VECTOR('',#6043,0.3);
#1994=VECTOR('',#6052,1.);
#1995=VECTOR('',#6053,1.);
#1996=VECTOR('',#6054,1.);
#1997=VECTOR('',#6055,1.);
#1998=VECTOR('',#6056,1.);
#1999=VECTOR('',#6057,1.);
#2000=VECTOR('',#6058,1.);
#2001=VECTOR('',#6059,1.);
#2002=VECTOR('',#6060,1.);
#2003=VECTOR('',#6063,1.);
#2004=VECTOR('',#6064,1.);
#2005=VECTOR('',#6067,1.);
#2006=VECTOR('',#6068,1.);
#2007=VECTOR('',#6071,1.);
#2008=VECTOR('',#6072,1.);
#2009=VECTOR('',#6075,1.);
#2010=VECTOR('',#6076,1.);
#2011=VECTOR('',#6079,1.);
#2012=VECTOR('',#6082,1.);
#2013=VECTOR('',#6083,1.);
#2014=VECTOR('',#6084,1.);
#2015=VECTOR('',#6085,1.);
#2016=VECTOR('',#6086,1.);
#2017=VECTOR('',#6087,1.);
#2018=VECTOR('',#6088,1.);
#2019=VECTOR('',#6089,1.);
#2020=VECTOR('',#6090,1.);
#2021=VECTOR('',#6091,1.);
#2022=VECTOR('',#6092,1.);
#2023=VECTOR('',#6093,1.);
#2024=VECTOR('',#6094,1.);
#2025=VECTOR('',#6095,1.);
#2026=VECTOR('',#6096,1.);
#2027=VECTOR('',#6105,0.275);
#2028=VECTOR('',#6110,0.275);
#2029=VECTOR('',#6115,0.51);
#2030=VECTOR('',#6120,1.);
#2031=VECTOR('',#6121,1.);
#2032=VECTOR('',#6122,1.);
#2033=VECTOR('',#6125,1.);
#2034=VECTOR('',#6126,1.);
#2035=VECTOR('',#6129,1.);
#2036=VECTOR('',#6130,1.);
#2037=VECTOR('',#6133,1.);
#2038=VECTOR('',#6140,0.31);
#2039=VECTOR('',#6147,0.31);
#2040=VECTOR('',#6152,1.);
#2041=VECTOR('',#6153,1.);
#2042=VECTOR('',#6154,1.);
#2043=VECTOR('',#6157,1.);
#2044=VECTOR('',#6158,1.);
#2045=VECTOR('',#6161,1.);
#2046=VECTOR('',#6162,1.);
#2047=VECTOR('',#6165,1.);
#2048=VECTOR('',#6170,1.);
#2049=VECTOR('',#6171,1.);
#2050=VECTOR('',#6172,1.);
#2051=VECTOR('',#6175,1.);
#2052=VECTOR('',#6176,1.);
#2053=VECTOR('',#6179,1.);
#2054=VECTOR('',#6180,1.);
#2055=VECTOR('',#6183,1.);
#2056=VECTOR('',#6188,1.);
#2057=VECTOR('',#6189,1.);
#2058=VECTOR('',#6192,1.);
#2059=VECTOR('',#6193,1.);
#2060=VECTOR('',#6196,1.);
#2061=VECTOR('',#6203,1.);
#2062=VECTOR('',#6206,1.);
#2063=VECTOR('',#6211,1.);
#2064=VECTOR('',#6214,1.);
#2065=VECTOR('',#6215,1.);
#2066=VECTOR('',#6216,1.);
#2067=VECTOR('',#6217,1.);
#2068=VECTOR('',#6218,1.);
#2069=VECTOR('',#6225,0.33);
#2070=VECTOR('',#6230,0.33);
#2071=VECTOR('',#6235,1.);
#2072=VECTOR('',#6236,1.);
#2073=VECTOR('',#6237,1.);
#2074=VECTOR('',#6242,0.210000000000001);
#2075=VECTOR('',#6249,1.);
#2076=VECTOR('',#6250,1.);
#2077=VECTOR('',#6251,1.);
#2078=VECTOR('',#6254,1.);
#2079=VECTOR('',#6255,1.);
#2080=VECTOR('',#6256,1.);
#2081=VECTOR('',#6257,1.);
#2082=VECTOR('',#6260,1.);
#2083=VECTOR('',#6261,1.);
#2084=VECTOR('',#6264,1.);
#2085=VECTOR('',#6265,1.);
#2086=VECTOR('',#6266,1.);
#2087=VECTOR('',#6271,0.21);
#2088=VECTOR('',#6278,1.);
#2089=VECTOR('',#6279,1.);
#2090=VECTOR('',#6280,1.);
#2091=VECTOR('',#6283,1.);
#2092=VECTOR('',#6284,1.);
#2093=VECTOR('',#6285,1.);
#2094=VECTOR('',#6286,1.);
#2095=VECTOR('',#6289,1.);
#2096=VECTOR('',#6290,1.);
#2097=VECTOR('',#6293,1.);
#2098=VECTOR('',#6294,1.);
#2099=VECTOR('',#6295,1.);
#2100=VECTOR('',#6298,1.);
#2101=VECTOR('',#6299,1.);
#2102=VECTOR('',#6300,1.);
#2103=VECTOR('',#6303,1.);
#2104=VECTOR('',#6304,1.);
#2105=VECTOR('',#6305,1.);
#2106=VECTOR('',#6308,1.);
#2107=VECTOR('',#6309,1.);
#2108=VECTOR('',#6312,1.);
#2109=VECTOR('',#6313,1.);
#2110=VECTOR('',#6316,1.);
#2111=VECTOR('',#6325,0.275);
#2112=VECTOR('',#6330,0.265);
#2113=VECTOR('',#6339,0.5);
#2114=VECTOR('',#6348,1.);
#2115=VECTOR('',#6349,1.);
#2116=VECTOR('',#6350,1.);
#2117=VECTOR('',#6351,1.);
#2118=VECTOR('',#6354,1.);
#2119=VECTOR('',#6355,1.);
#2120=VECTOR('',#6356,1.);
#2121=VECTOR('',#6359,1.);
#2122=VECTOR('',#6360,1.);
#2123=VECTOR('',#6361,1.);
#2124=VECTOR('',#6364,1.);
#2125=VECTOR('',#6365,1.);
#2126=VECTOR('',#6366,1.);
#2127=VECTOR('',#6369,1.);
#2128=VECTOR('',#6370,1.);
#2129=VECTOR('',#6371,1.);
#2130=VECTOR('',#6374,1.);
#2131=VECTOR('',#6375,1.);
#2132=VECTOR('',#6392,0.4);
#2133=VECTOR('',#6397,0.425);
#2134=VECTOR('',#6402,0.41);
#2135=VECTOR('',#6411,0.26);
#2136=VECTOR('',#6414,0.25);
#2137=VECTOR('',#6421,0.3);
#2138=VECTOR('',#6428,0.3);
#2139=VECTOR('',#6435,0.33);
#2140=VECTOR('',#6442,0.33);
#2141=VECTOR('',#6449,0.33);
#2142=VECTOR('',#6456,0.33);
#2143=VECTOR('',#6463,0.33);
#2144=VECTOR('',#6470,0.33);
#2145=VECTOR('',#6477,0.34);
#2146=VECTOR('',#6484,0.34);
#2147=VECTOR('',#6491,0.34);
#2148=VECTOR('',#6498,0.34);
#2149=VECTOR('',#6505,0.34);
#2150=VECTOR('',#6512,0.34);
#2151=VECTOR('',#6519,0.34);
#2152=VECTOR('',#6526,0.34);
#2153=VECTOR('',#6533,0.34);
#2154=VECTOR('',#6540,0.34);
#2155=VECTOR('',#6547,0.34);
#2156=VECTOR('',#6554,0.34);
#2157=VECTOR('',#6561,0.34);
#2158=VECTOR('',#6568,0.34);
#2159=VECTOR('',#6575,0.34);
#2160=VECTOR('',#6582,0.34);
#2161=VECTOR('',#6589,0.34);
#2162=VECTOR('',#6596,0.34);
#2163=VECTOR('',#6603,0.34);
#2164=VECTOR('',#6610,0.34);
#2165=VECTOR('',#6615,1.);
#2166=VECTOR('',#6616,1.);
#2167=VECTOR('',#6617,1.);
#2168=VECTOR('',#6618,1.);
#2169=VECTOR('',#6621,1.);
#2170=VECTOR('',#6622,1.);
#2171=VECTOR('',#6623,1.);
#2172=VECTOR('',#6626,1.);
#2173=VECTOR('',#6627,1.);
#2174=VECTOR('',#6628,1.);
#2175=VECTOR('',#6631,1.);
#2176=VECTOR('',#6632,1.);
#2177=VECTOR('',#6643,0.425);
#2178=VECTOR('',#6650,0.425);
#2179=VECTOR('',#6655,1.);
#2180=VECTOR('',#6656,1.);
#2181=VECTOR('',#6657,1.);
#2182=VECTOR('',#6658,1.);
#2183=VECTOR('',#6661,1.);
#2184=VECTOR('',#6662,1.);
#2185=VECTOR('',#6663,1.);
#2186=VECTOR('',#6666,1.);
#2187=VECTOR('',#6667,1.);
#2188=VECTOR('',#6668,1.);
#2189=VECTOR('',#6671,1.);
#2190=VECTOR('',#6672,1.);
#2191=VECTOR('',#6683,0.3);
#2192=VECTOR('',#6690,0.27);
#2193=VECTOR('',#6697,0.576175134594813);
#2194=VECTOR('',#6700,1.);
#2195=VECTOR('',#6701,1.);
#2196=VECTOR('',#6702,1.);
#2197=VECTOR('',#6705,1.);
#2198=VECTOR('',#6706,1.);
#2199=VECTOR('',#6709,1.);
#2200=VECTOR('',#6710,1.);
#2201=VECTOR('',#6713,1.);
#2202=VECTOR('',#6714,1.);
#2203=VECTOR('',#6717,1.);
#2204=VECTOR('',#6718,1.);
#2205=VECTOR('',#6721,1.);
#2206=VECTOR('',#6730,0.576175134594813);
#2207=VECTOR('',#6737,0.576175134594813);
#2208=VECTOR('',#6740,1.);
#2209=VECTOR('',#6741,1.);
#2210=VECTOR('',#6744,1.);
#2211=VECTOR('',#6747,1.);
#2212=VECTOR('',#6752,0.3);
#2213=VECTOR('',#6757,1.);
#2214=VECTOR('',#6760,1.);
#2215=VECTOR('',#6773,0.4);
#2216=VECTOR('',#6782,0.8);
#2217=VECTOR('',#6799,0.3);
#2218=VECTOR('',#6804,0.26);
#2219=VECTOR('',#6813,1.);
#2220=VECTOR('',#6816,1.);
#2221=VECTOR('',#6817,1.);
#2222=VECTOR('',#6818,1.);
#2223=VECTOR('',#6823,1.);
#2224=VECTOR('',#6826,0.3);
#2225=VECTOR('',#6831,1.);
#2226=VECTOR('',#6840,1.);
#2227=VECTOR('',#6841,1.);
#2228=VECTOR('',#6856,1.);
#2229=VECTOR('',#6857,1.);
#2230=VECTOR('',#6858,1.);
#2231=VECTOR('',#6859,1.);
#2232=VECTOR('',#6862,1.);
#2233=VECTOR('',#6863,1.);
#2234=VECTOR('',#6864,1.);
#2235=VECTOR('',#6867,1.);
#2236=VECTOR('',#6868,1.);
#2237=VECTOR('',#6869,1.);
#2238=VECTOR('',#6872,1.);
#2239=VECTOR('',#6873,1.);
#2240=VECTOR('',#6874,1.);
#2241=VECTOR('',#6877,1.);
#2242=VECTOR('',#6878,1.);
#2243=VECTOR('',#6879,1.);
#2244=VECTOR('',#6882,1.);
#2245=VECTOR('',#6883,1.);
#2246=VECTOR('',#6900,0.625);
#2247=VECTOR('',#6905,0.65);
#2248=VECTOR('',#6910,0.635);
#2249=VECTOR('',#6919,0.41);
#2250=VECTOR('',#6922,0.4);
#2251=VECTOR('',#6931,0.275);
#2252=VECTOR('',#6938,0.31);
#2253=VECTOR('',#6943,1.);
#2254=VECTOR('',#6946,1.);
#2255=VECTOR('',#6951,1.);
#2256=VECTOR('',#6954,1.);
#2257=VECTOR('',#6957,1.);
#2258=VECTOR('',#6958,1.);
#2259=VECTOR('',#6961,1.);
#2260=VECTOR('',#6966,1.);
#2261=VECTOR('',#6971,0.31);
#2262=VECTOR('',#6978,0.31);
#2263=VECTOR('',#6983,1.);
#2264=VECTOR('',#6984,1.);
#2265=VECTOR('',#6985,1.);
#2266=VECTOR('',#6986,1.);
#2267=VECTOR('',#6989,1.);
#2268=VECTOR('',#6990,1.);
#2269=VECTOR('',#6991,1.);
#2270=VECTOR('',#6992,1.);
#2271=VECTOR('',#6995,1.);
#2272=VECTOR('',#6996,1.);
#2273=VECTOR('',#6997,1.);
#2274=VECTOR('',#7000,1.);
#2275=VECTOR('',#7001,1.);
#2276=VECTOR('',#7004,1.);
#2277=VECTOR('',#7005,1.);
#2278=VECTOR('',#7008,1.);
#2279=VECTOR('',#7011,1.);
#2280=VECTOR('',#7012,1.);
#2281=VECTOR('',#7013,1.);
#2282=VECTOR('',#7016,1.);
#2283=VECTOR('',#7017,1.);
#2284=VECTOR('',#7022,1.);
#2285=VECTOR('',#7023,1.);
#2286=VECTOR('',#7028,0.6);
#2287=VECTOR('',#7037,1.);
#2288=VECTOR('',#7038,1.);
#2289=VECTOR('',#7039,1.);
#2290=VECTOR('',#7040,1.);
#2291=VECTOR('',#7043,1.);
#2292=VECTOR('',#7044,1.);
#2293=VECTOR('',#7047,1.);
#2294=VECTOR('',#7048,1.);
#2295=VECTOR('',#7051,1.);
#2296=VECTOR('',#7052,1.);
#2297=VECTOR('',#7055,1.);
#2298=VECTOR('',#7064,0.21);
#2299=VECTOR('',#7073,0.7);
#2300=VECTOR('',#7084,1.);
#2301=VECTOR('',#7085,1.);
#2302=VECTOR('',#7086,1.);
#2303=VECTOR('',#7087,1.);
#2304=VECTOR('',#7090,1.);
#2305=VECTOR('',#7091,1.);
#2306=VECTOR('',#7092,1.);
#2307=VECTOR('',#7095,1.);
#2308=VECTOR('',#7096,1.);
#2309=VECTOR('',#7097,1.);
#2310=VECTOR('',#7100,1.);
#2311=VECTOR('',#7101,1.);
#2312=VECTOR('',#7102,1.);
#2313=VECTOR('',#7105,1.);
#2314=VECTOR('',#7106,1.);
#2315=VECTOR('',#7107,1.);
#2316=VECTOR('',#7110,1.);
#2317=VECTOR('',#7111,1.);
#2318=VECTOR('',#7128,0.4);
#2319=VECTOR('',#7133,0.425);
#2320=VECTOR('',#7138,0.41);
#2321=VECTOR('',#7147,0.26);
#2322=VECTOR('',#7150,0.25);
#2323=VECTOR('',#7159,0.31);
#2324=VECTOR('',#7166,0.31);
#2325=VECTOR('',#7171,1.);
#2326=VECTOR('',#7174,1.);
#2327=VECTOR('',#7179,1.);
#2328=VECTOR('',#7180,1.);
#2329=VECTOR('',#7181,1.);
#2330=VECTOR('',#7184,1.);
#2331=VECTOR('',#7189,1.);
#2332=VECTOR('',#7190,1.);
#2333=VECTOR('',#7207,0.34);
#2334=VECTOR('',#7216,0.31);
#2335=VECTOR('',#7223,0.31);
#2336=VECTOR('',#7228,1.);
#2337=VECTOR('',#7229,1.);
#2338=VECTOR('',#7230,1.);
#2339=VECTOR('',#7231,1.);
#2340=VECTOR('',#7234,1.);
#2341=VECTOR('',#7235,1.);
#2342=VECTOR('',#7236,1.);
#2343=VECTOR('',#7237,1.);
#2344=VECTOR('',#7240,1.);
#2345=VECTOR('',#7241,1.);
#2346=VECTOR('',#7242,1.);
#2347=VECTOR('',#7243,1.);
#2348=VECTOR('',#7244,1.);
#2349=VECTOR('',#7245,1.);
#2350=VECTOR('',#7248,1.);
#2351=VECTOR('',#7249,1.);
#2352=VECTOR('',#7250,1.);
#2353=VECTOR('',#7253,1.);
#2354=VECTOR('',#7254,1.);
#2355=VECTOR('',#7257,1.);
#2356=VECTOR('',#7262,1.);
#2357=VECTOR('',#7263,1.);
#2358=VECTOR('',#7264,1.);
#2359=VECTOR('',#7269,1.);
#2360=VECTOR('',#7276,0.5);
#2361=VECTOR('',#7285,0.4);
#2362=VECTOR('',#7292,0.36);
#2363=VECTOR('',#7299,0.734027674973257);
#2364=VECTOR('',#7302,1.);
#2365=VECTOR('',#7303,1.);
#2366=VECTOR('',#7304,1.);
#2367=VECTOR('',#7307,1.);
#2368=VECTOR('',#7308,1.);
#2369=VECTOR('',#7311,1.);
#2370=VECTOR('',#7312,1.);
#2371=VECTOR('',#7315,1.);
#2372=VECTOR('',#7316,1.);
#2373=VECTOR('',#7319,1.);
#2374=VECTOR('',#7320,1.);
#2375=VECTOR('',#7323,1.);
#2376=VECTOR('',#7332,0.734027674973257);
#2377=VECTOR('',#7339,0.734027674973257);
#2378=VECTOR('',#7342,1.);
#2379=VECTOR('',#7343,1.);
#2380=VECTOR('',#7346,1.);
#2381=VECTOR('',#7349,1.);
#2382=VECTOR('',#7354,0.4);
#2383=VECTOR('',#7359,1.);
#2384=VECTOR('',#7362,1.);
#2385=VECTOR('',#7375,1.);
#2386=VECTOR('',#7386,0.08);
#2387=VECTOR('',#7395,0.475);
#2388=VECTOR('',#7400,0.5);
#2389=VECTOR('',#7409,0.3);
#2390=VECTOR('',#7410,0.3);
#2391=VECTOR('',#7415,0.255);
#2392=VECTOR('',#7424,0.32);
#2393=VECTOR('',#7431,0.6);
#2394=VECTOR('',#7444,0.31);
#2395=VECTOR('',#7451,0.5);
#2396=VECTOR('',#7470,1.);
#2397=VECTOR('',#7473,1.);
#2398=VECTOR('',#7474,1.);
#2399=VECTOR('',#7475,1.);
#2400=VECTOR('',#7480,0.08);
#2401=VERTEX_POINT('',#7579);
#2402=VERTEX_POINT('',#7580);
#2403=VERTEX_POINT('',#7582);
#2404=VERTEX_POINT('',#7584);
#2405=VERTEX_POINT('',#7586);
#2406=VERTEX_POINT('',#7588);
#2407=VERTEX_POINT('',#7594);
#2408=VERTEX_POINT('',#7596);
#2409=VERTEX_POINT('',#7598);
#2410=VERTEX_POINT('',#7600);
#2411=VERTEX_POINT('',#7602);
#2412=VERTEX_POINT('',#7604);
#2413=VERTEX_POINT('',#7606);
#2414=VERTEX_POINT('',#7608);
#2415=VERTEX_POINT('',#7612);
#2416=VERTEX_POINT('',#7616);
#2417=VERTEX_POINT('',#7620);
#2418=VERTEX_POINT('',#7624);
#2419=VERTEX_POINT('',#7630);
#2420=VERTEX_POINT('',#7632);
#2421=VERTEX_POINT('',#7635);
#2422=VERTEX_POINT('',#7636);
#2423=VERTEX_POINT('',#7638);
#2424=VERTEX_POINT('',#7640);
#2425=VERTEX_POINT('',#7643);
#2426=VERTEX_POINT('',#7644);
#2427=VERTEX_POINT('',#7646);
#2428=VERTEX_POINT('',#7648);
#2429=VERTEX_POINT('',#7651);
#2430=VERTEX_POINT('',#7652);
#2431=VERTEX_POINT('',#7654);
#2432=VERTEX_POINT('',#7656);
#2433=VERTEX_POINT('',#7659);
#2434=VERTEX_POINT('',#7661);
#2435=VERTEX_POINT('',#7664);
#2436=VERTEX_POINT('',#7668);
#2437=VERTEX_POINT('',#7672);
#2438=VERTEX_POINT('',#7674);
#2439=VERTEX_POINT('',#7678);
#2440=VERTEX_POINT('',#7680);
#2441=VERTEX_POINT('',#7684);
#2442=VERTEX_POINT('',#7688);
#2443=VERTEX_POINT('',#7695);
#2444=VERTEX_POINT('',#7697);
#2445=VERTEX_POINT('',#7701);
#2446=VERTEX_POINT('',#7703);
#2447=VERTEX_POINT('',#7707);
#2448=VERTEX_POINT('',#7709);
#2449=VERTEX_POINT('',#7713);
#2450=VERTEX_POINT('',#7717);
#2451=VERTEX_POINT('',#7724);
#2452=VERTEX_POINT('',#7726);
#2453=VERTEX_POINT('',#7730);
#2454=VERTEX_POINT('',#7734);
#2455=VERTEX_POINT('',#7741);
#2456=VERTEX_POINT('',#7745);
#2457=VERTEX_POINT('',#7753);
#2458=VERTEX_POINT('',#7754);
#2459=VERTEX_POINT('',#7756);
#2460=VERTEX_POINT('',#7758);
#2461=VERTEX_POINT('',#7764);
#2462=VERTEX_POINT('',#7766);
#2463=VERTEX_POINT('',#7768);
#2464=VERTEX_POINT('',#7770);
#2465=VERTEX_POINT('',#7773);
#2466=VERTEX_POINT('',#7775);
#2467=VERTEX_POINT('',#7778);
#2468=VERTEX_POINT('',#7782);
#2469=VERTEX_POINT('',#7786);
#2470=VERTEX_POINT('',#7788);
#2471=VERTEX_POINT('',#7792);
#2472=VERTEX_POINT('',#7794);
#2473=VERTEX_POINT('',#7799);
#2474=VERTEX_POINT('',#7801);
#2475=VERTEX_POINT('',#7805);
#2476=VERTEX_POINT('',#7806);
#2477=VERTEX_POINT('',#7808);
#2478=VERTEX_POINT('',#7810);
#2479=VERTEX_POINT('',#7817);
#2480=VERTEX_POINT('',#7819);
#2481=VERTEX_POINT('',#7823);
#2482=VERTEX_POINT('',#7825);
#2483=VERTEX_POINT('',#7830);
#2484=VERTEX_POINT('',#7832);
#2485=VERTEX_POINT('',#7836);
#2486=VERTEX_POINT('',#7837);
#2487=VERTEX_POINT('',#7839);
#2488=VERTEX_POINT('',#7841);
#2489=VERTEX_POINT('',#7848);
#2490=VERTEX_POINT('',#7850);
#2491=VERTEX_POINT('',#7854);
#2492=VERTEX_POINT('',#7856);
#2493=VERTEX_POINT('',#7860);
#2494=VERTEX_POINT('',#7862);
#2495=VERTEX_POINT('',#7866);
#2496=VERTEX_POINT('',#7870);
#2497=VERTEX_POINT('',#7878);
#2498=VERTEX_POINT('',#7880);
#2499=VERTEX_POINT('',#7884);
#2500=VERTEX_POINT('',#7888);
#2501=VERTEX_POINT('',#7891);
#2502=VERTEX_POINT('',#7897);
#2503=VERTEX_POINT('',#7898);
#2504=VERTEX_POINT('',#7900);
#2505=VERTEX_POINT('',#7902);
#2506=VERTEX_POINT('',#7906);
#2507=VERTEX_POINT('',#7908);
#2508=VERTEX_POINT('',#7912);
#2509=VERTEX_POINT('',#7914);
#2510=VERTEX_POINT('',#7918);
#2511=VERTEX_POINT('',#7920);
#2512=VERTEX_POINT('',#7924);
#2513=VERTEX_POINT('',#7926);
#2514=VERTEX_POINT('',#7935);
#2515=VERTEX_POINT('',#7938);
#2516=VERTEX_POINT('',#7941);
#2517=VERTEX_POINT('',#7945);
#2518=VERTEX_POINT('',#7949);
#2519=VERTEX_POINT('',#7953);
#2520=VERTEX_POINT('',#7956);
#2521=VERTEX_POINT('',#7963);
#2522=VERTEX_POINT('',#7965);
#2523=VERTEX_POINT('',#7969);
#2524=VERTEX_POINT('',#7971);
#2525=VERTEX_POINT('',#7975);
#2526=VERTEX_POINT('',#7977);
#2527=VERTEX_POINT('',#7981);
#2528=VERTEX_POINT('',#7983);
#2529=VERTEX_POINT('',#7987);
#2530=VERTEX_POINT('',#7989);
#2531=VERTEX_POINT('',#7993);
#2532=VERTEX_POINT('',#7995);
#2533=VERTEX_POINT('',#7999);
#2534=VERTEX_POINT('',#8001);
#2535=VERTEX_POINT('',#8005);
#2536=VERTEX_POINT('',#8007);
#2537=VERTEX_POINT('',#8011);
#2538=VERTEX_POINT('',#8013);
#2539=VERTEX_POINT('',#8017);
#2540=VERTEX_POINT('',#8019);
#2541=VERTEX_POINT('',#8023);
#2542=VERTEX_POINT('',#8025);
#2543=VERTEX_POINT('',#8029);
#2544=VERTEX_POINT('',#8031);
#2545=VERTEX_POINT('',#8035);
#2546=VERTEX_POINT('',#8037);
#2547=VERTEX_POINT('',#8041);
#2548=VERTEX_POINT('',#8043);
#2549=VERTEX_POINT('',#8047);
#2550=VERTEX_POINT('',#8049);
#2551=VERTEX_POINT('',#8053);
#2552=VERTEX_POINT('',#8055);
#2553=VERTEX_POINT('',#8059);
#2554=VERTEX_POINT('',#8061);
#2555=VERTEX_POINT('',#8065);
#2556=VERTEX_POINT('',#8067);
#2557=VERTEX_POINT('',#8071);
#2558=VERTEX_POINT('',#8073);
#2559=VERTEX_POINT('',#8077);
#2560=VERTEX_POINT('',#8079);
#2561=VERTEX_POINT('',#8083);
#2562=VERTEX_POINT('',#8085);
#2563=VERTEX_POINT('',#8089);
#2564=VERTEX_POINT('',#8091);
#2565=VERTEX_POINT('',#8095);
#2566=VERTEX_POINT('',#8097);
#2567=VERTEX_POINT('',#8101);
#2568=VERTEX_POINT('',#8103);
#2569=VERTEX_POINT('',#8107);
#2570=VERTEX_POINT('',#8109);
#2571=VERTEX_POINT('',#8113);
#2572=VERTEX_POINT('',#8115);
#2573=VERTEX_POINT('',#8119);
#2574=VERTEX_POINT('',#8121);
#2575=VERTEX_POINT('',#8125);
#2576=VERTEX_POINT('',#8127);
#2577=VERTEX_POINT('',#8131);
#2578=VERTEX_POINT('',#8132);
#2579=VERTEX_POINT('',#8134);
#2580=VERTEX_POINT('',#8136);
#2581=VERTEX_POINT('',#8140);
#2582=VERTEX_POINT('',#8142);
#2583=VERTEX_POINT('',#8146);
#2584=VERTEX_POINT('',#8148);
#2585=VERTEX_POINT('',#8158);
#2586=VERTEX_POINT('',#8160);
#2587=VERTEX_POINT('',#8164);
#2588=VERTEX_POINT('',#8166);
#2589=VERTEX_POINT('',#8170);
#2590=VERTEX_POINT('',#8171);
#2591=VERTEX_POINT('',#8173);
#2592=VERTEX_POINT('',#8175);
#2593=VERTEX_POINT('',#8179);
#2594=VERTEX_POINT('',#8181);
#2595=VERTEX_POINT('',#8185);
#2596=VERTEX_POINT('',#8187);
#2597=VERTEX_POINT('',#8197);
#2598=VERTEX_POINT('',#8199);
#2599=VERTEX_POINT('',#8203);
#2600=VERTEX_POINT('',#8208);
#2601=VERTEX_POINT('',#8210);
#2602=VERTEX_POINT('',#8212);
#2603=VERTEX_POINT('',#8216);
#2604=VERTEX_POINT('',#8220);
#2605=VERTEX_POINT('',#8224);
#2606=VERTEX_POINT('',#8228);
#2607=VERTEX_POINT('',#8236);
#2608=VERTEX_POINT('',#8238);
#2609=VERTEX_POINT('',#8242);
#2610=VERTEX_POINT('',#8246);
#2611=VERTEX_POINT('',#8250);
#2612=VERTEX_POINT('',#8254);
#2613=VERTEX_POINT('',#8263);
#2614=VERTEX_POINT('',#8264);
#2615=VERTEX_POINT('',#8268);
#2616=VERTEX_POINT('',#8272);
#2617=VERTEX_POINT('',#8275);
#2618=VERTEX_POINT('',#8279);
#2619=VERTEX_POINT('',#8283);
#2620=VERTEX_POINT('',#8291);
#2621=VERTEX_POINT('',#8293);
#2622=VERTEX_POINT('',#8295);
#2623=VERTEX_POINT('',#8299);
#2624=VERTEX_POINT('',#8303);
#2625=VERTEX_POINT('',#8307);
#2626=VERTEX_POINT('',#8311);
#2627=VERTEX_POINT('',#8326);
#2628=VERTEX_POINT('',#8328);
#2629=VERTEX_POINT('',#8340);
#2630=VERTEX_POINT('',#8342);
#2631=VERTEX_POINT('',#8347);
#2632=VERTEX_POINT('',#8349);
#2633=VERTEX_POINT('',#8356);
#2634=VERTEX_POINT('',#8359);
#2635=VERTEX_POINT('',#8363);
#2636=VERTEX_POINT('',#8369);
#2637=VERTEX_POINT('',#8370);
#2638=VERTEX_POINT('',#8374);
#2639=VERTEX_POINT('',#8376);
#2640=VERTEX_POINT('',#8380);
#2641=VERTEX_POINT('',#8382);
#2642=VERTEX_POINT('',#8388);
#2643=VERTEX_POINT('',#8390);
#2644=VERTEX_POINT('',#8392);
#2645=VERTEX_POINT('',#8394);
#2646=VERTEX_POINT('',#8397);
#2647=VERTEX_POINT('',#8399);
#2648=VERTEX_POINT('',#8403);
#2649=VERTEX_POINT('',#8410);
#2650=VERTEX_POINT('',#8422);
#2651=VERTEX_POINT('',#8423);
#2652=VERTEX_POINT('',#8425);
#2653=VERTEX_POINT('',#8427);
#2654=VERTEX_POINT('',#8431);
#2655=VERTEX_POINT('',#8433);
#2656=VERTEX_POINT('',#8437);
#2657=VERTEX_POINT('',#8439);
#2658=VERTEX_POINT('',#8443);
#2659=VERTEX_POINT('',#8445);
#2660=VERTEX_POINT('',#8449);
#2661=VERTEX_POINT('',#8451);
#2662=VERTEX_POINT('',#8460);
#2663=VERTEX_POINT('',#8463);
#2664=VERTEX_POINT('',#8466);
#2665=VERTEX_POINT('',#8470);
#2666=VERTEX_POINT('',#8474);
#2667=VERTEX_POINT('',#8478);
#2668=VERTEX_POINT('',#8481);
#2669=VERTEX_POINT('',#8489);
#2670=VERTEX_POINT('',#8491);
#2671=VERTEX_POINT('',#8495);
#2672=VERTEX_POINT('',#8497);
#2673=VERTEX_POINT('',#8501);
#2674=VERTEX_POINT('',#8502);
#2675=VERTEX_POINT('',#8504);
#2676=VERTEX_POINT('',#8506);
#2677=VERTEX_POINT('',#8510);
#2678=VERTEX_POINT('',#8512);
#2679=VERTEX_POINT('',#8516);
#2680=VERTEX_POINT('',#8520);
#2681=VERTEX_POINT('',#8526);
#2682=VERTEX_POINT('',#8528);
#2683=VERTEX_POINT('',#8532);
#2684=VERTEX_POINT('',#8534);
#2685=VERTEX_POINT('',#8538);
#2686=VERTEX_POINT('',#8539);
#2687=VERTEX_POINT('',#8541);
#2688=VERTEX_POINT('',#8543);
#2689=VERTEX_POINT('',#8547);
#2690=VERTEX_POINT('',#8548);
#2691=VERTEX_POINT('',#8550);
#2692=VERTEX_POINT('',#8552);
#2693=VERTEX_POINT('',#8556);
#2694=VERTEX_POINT('',#8557);
#2695=VERTEX_POINT('',#8565);
#2696=VERTEX_POINT('',#8566);
#2697=VERTEX_POINT('',#8568);
#2698=VERTEX_POINT('',#8570);
#2699=VERTEX_POINT('',#8574);
#2700=VERTEX_POINT('',#8576);
#2701=VERTEX_POINT('',#8580);
#2702=VERTEX_POINT('',#8582);
#2703=VERTEX_POINT('',#8589);
#2704=VERTEX_POINT('',#8591);
#2705=VERTEX_POINT('',#8597);
#2706=VERTEX_POINT('',#8599);
#2707=VERTEX_POINT('',#8601);
#2708=VERTEX_POINT('',#8605);
#2709=VERTEX_POINT('',#8609);
#2710=VERTEX_POINT('',#8613);
#2711=VERTEX_POINT('',#8621);
#2712=VERTEX_POINT('',#8623);
#2713=VERTEX_POINT('',#8628);
#2714=VERTEX_POINT('',#8630);
#2715=VERTEX_POINT('',#8637);
#2716=VERTEX_POINT('',#8638);
#2717=VERTEX_POINT('',#8640);
#2718=VERTEX_POINT('',#8642);
#2719=VERTEX_POINT('',#8646);
#2720=VERTEX_POINT('',#8648);
#2721=VERTEX_POINT('',#8652);
#2722=VERTEX_POINT('',#8654);
#2723=VERTEX_POINT('',#8658);
#2724=VERTEX_POINT('',#8660);
#2725=VERTEX_POINT('',#8664);
#2726=VERTEX_POINT('',#8666);
#2727=VERTEX_POINT('',#8675);
#2728=VERTEX_POINT('',#8678);
#2729=VERTEX_POINT('',#8681);
#2730=VERTEX_POINT('',#8685);
#2731=VERTEX_POINT('',#8689);
#2732=VERTEX_POINT('',#8693);
#2733=VERTEX_POINT('',#8696);
#2734=VERTEX_POINT('',#8704);
#2735=VERTEX_POINT('',#8706);
#2736=VERTEX_POINT('',#8710);
#2737=VERTEX_POINT('',#8712);
#2738=VERTEX_POINT('',#8716);
#2739=VERTEX_POINT('',#8717);
#2740=VERTEX_POINT('',#8719);
#2741=VERTEX_POINT('',#8721);
#2742=VERTEX_POINT('',#8725);
#2743=VERTEX_POINT('',#8727);
#2744=VERTEX_POINT('',#8731);
#2745=VERTEX_POINT('',#8735);
#2746=VERTEX_POINT('',#8745);
#2747=VERTEX_POINT('',#8747);
#2748=VERTEX_POINT('',#8752);
#2749=VERTEX_POINT('',#8754);
#2750=VERTEX_POINT('',#8758);
#2751=VERTEX_POINT('',#8760);
#2752=VERTEX_POINT('',#8764);
#2753=VERTEX_POINT('',#8765);
#2754=VERTEX_POINT('',#8767);
#2755=VERTEX_POINT('',#8769);
#2756=VERTEX_POINT('',#8773);
#2757=VERTEX_POINT('',#8774);
#2758=VERTEX_POINT('',#8776);
#2759=VERTEX_POINT('',#8778);
#2760=VERTEX_POINT('',#8782);
#2761=VERTEX_POINT('',#8785);
#2762=VERTEX_POINT('',#8787);
#2763=VERTEX_POINT('',#8789);
#2764=VERTEX_POINT('',#8793);
#2765=VERTEX_POINT('',#8794);
#2766=VERTEX_POINT('',#8799);
#2767=VERTEX_POINT('',#8804);
#2768=VERTEX_POINT('',#8808);
#2769=VERTEX_POINT('',#8816);
#2770=VERTEX_POINT('',#8822);
#2771=VERTEX_POINT('',#8824);
#2772=VERTEX_POINT('',#8828);
#2773=VERTEX_POINT('',#8833);
#2774=VERTEX_POINT('',#8835);
#2775=VERTEX_POINT('',#8837);
#2776=VERTEX_POINT('',#8841);
#2777=VERTEX_POINT('',#8845);
#2778=VERTEX_POINT('',#8849);
#2779=VERTEX_POINT('',#8853);
#2780=VERTEX_POINT('',#8861);
#2781=VERTEX_POINT('',#8863);
#2782=VERTEX_POINT('',#8867);
#2783=VERTEX_POINT('',#8871);
#2784=VERTEX_POINT('',#8875);
#2785=VERTEX_POINT('',#8879);
#2786=VERTEX_POINT('',#8888);
#2787=VERTEX_POINT('',#8889);
#2788=VERTEX_POINT('',#8893);
#2789=VERTEX_POINT('',#8897);
#2790=VERTEX_POINT('',#8900);
#2791=VERTEX_POINT('',#8904);
#2792=VERTEX_POINT('',#8908);
#2793=VERTEX_POINT('',#8916);
#2794=VERTEX_POINT('',#8918);
#2795=VERTEX_POINT('',#8920);
#2796=VERTEX_POINT('',#8924);
#2797=VERTEX_POINT('',#8928);
#2798=VERTEX_POINT('',#8932);
#2799=VERTEX_POINT('',#8936);
#2800=VERTEX_POINT('',#8951);
#2801=VERTEX_POINT('',#8953);
#2802=VERTEX_POINT('',#8965);
#2803=VERTEX_POINT('',#8967);
#2804=VERTEX_POINT('',#8974);
#2805=VERTEX_POINT('',#8975);
#2806=VERTEX_POINT('',#8986);
#2807=VERTEX_POINT('',#9022);
#2808=VERTEX_POINT('',#9052);
#2809=VERTEX_POINT('',#9055);
#2810=VERTEX_POINT('',#9059);
#2811=VERTEX_POINT('',#9063);
#2812=VERTEX_POINT('',#9066);
#2813=VERTEX_POINT('',#9071);
#2814=VERTEX_POINT('',#9077);
#2815=VERTEX_POINT('',#9079);
#2816=VERTEX_POINT('',#9083);
#2817=VERTEX_POINT('',#9085);
#2818=VERTEX_POINT('',#9092);
#2819=VERTEX_POINT('',#9094);
#2820=VERTEX_POINT('',#9098);
#2821=VERTEX_POINT('',#9100);
#2822=VERTEX_POINT('',#9107);
#2823=VERTEX_POINT('',#9110);
#2824=VERTEX_POINT('',#9111);
#2825=VERTEX_POINT('',#9165);
#2826=VERTEX_POINT('',#9166);
#2827=VERTEX_POINT('',#9170);
#2828=VERTEX_POINT('',#9172);
#2829=VERTEX_POINT('',#9176);
#2830=EDGE_CURVE('',#2401,#2402,#1581,.T.);
#2831=EDGE_CURVE('',#2403,#2401,#1383,.T.);
#2832=EDGE_CURVE('',#2403,#2404,#1582,.T.);
#2833=EDGE_CURVE('',#2405,#2404,#1384,.T.);
#2834=EDGE_CURVE('',#2405,#2406,#1583,.T.);
#2835=EDGE_CURVE('',#2406,#2406,#1385,.T.);
#2836=EDGE_CURVE('',#2402,#2405,#1386,.T.);
#2837=EDGE_CURVE('',#2404,#2407,#1584,.T.);
#2838=EDGE_CURVE('',#2407,#2408,#1585,.T.);
#2839=EDGE_CURVE('',#2409,#2408,#1586,.T.);
#2840=EDGE_CURVE('',#2410,#2409,#1587,.T.);
#2841=EDGE_CURVE('',#2410,#2411,#1588,.T.);
#2842=EDGE_CURVE('',#2411,#2412,#1589,.T.);
#2843=EDGE_CURVE('',#2413,#2412,#1590,.T.);
#2844=EDGE_CURVE('',#2413,#2414,#1591,.T.);
#2845=EDGE_CURVE('',#2414,#2402,#1592,.T.);
#2846=EDGE_CURVE('',#2415,#2414,#1593,.T.);
#2847=EDGE_CURVE('',#2401,#2415,#1594,.T.);
#2848=EDGE_CURVE('',#2416,#2403,#1595,.T.);
#2849=EDGE_CURVE('',#2416,#2407,#1596,.T.);
#2850=EDGE_CURVE('',#2417,#2416,#1597,.T.);
#2851=EDGE_CURVE('',#2408,#2417,#1598,.T.);
#2852=EDGE_CURVE('',#2418,#2413,#1599,.T.);
#2853=EDGE_CURVE('',#2415,#2418,#1600,.T.);
#2854=EDGE_CURVE('',#2417,#2418,#1601,.T.);
#2855=EDGE_CURVE('',#2412,#2419,#1602,.T.);
#2856=EDGE_CURVE('',#2419,#2420,#1603,.T.);
#2857=EDGE_CURVE('',#2420,#2409,#1604,.T.);
#2858=EDGE_CURVE('',#2421,#2422,#1605,.T.);
#2859=EDGE_CURVE('',#2422,#2423,#1606,.T.);
#2860=EDGE_CURVE('',#2423,#2424,#1607,.T.);
#2861=EDGE_CURVE('',#2424,#2421,#1608,.T.);
#2862=EDGE_CURVE('',#2425,#2426,#1609,.T.);
#2863=EDGE_CURVE('',#2426,#2427,#1610,.T.);
#2864=EDGE_CURVE('',#2427,#2428,#1611,.T.);
#2865=EDGE_CURVE('',#2428,#2425,#1612,.T.);
#2866=EDGE_CURVE('',#2429,#2430,#1613,.T.);
#2867=EDGE_CURVE('',#2430,#2431,#1614,.T.);
#2868=EDGE_CURVE('',#2431,#2432,#1615,.T.);
#2869=EDGE_CURVE('',#2432,#2429,#1616,.T.);
#2870=EDGE_CURVE('',#2433,#2433,#1387,.T.);
#2871=EDGE_CURVE('',#2434,#2434,#1388,.T.);
#2872=EDGE_CURVE('',#2435,#2435,#1389,.T.);
#2873=EDGE_CURVE('',#2435,#2434,#1617,.T.);
#2874=EDGE_CURVE('',#2436,#2436,#1390,.T.);
#2875=EDGE_CURVE('',#2436,#2433,#1618,.T.);
#2876=EDGE_CURVE('',#2437,#2437,#1391,.T.);
#2877=EDGE_CURVE('',#2437,#2438,#1619,.T.);
#2878=EDGE_CURVE('',#2438,#2438,#1392,.T.);
#2879=EDGE_CURVE('',#2430,#2439,#1620,.T.);
#2880=EDGE_CURVE('',#2439,#2440,#1621,.T.);
#2881=EDGE_CURVE('',#2440,#2431,#1622,.T.);
#2882=EDGE_CURVE('',#2441,#2429,#1623,.T.);
#2883=EDGE_CURVE('',#2439,#2441,#1624,.T.);
#2884=EDGE_CURVE('',#2440,#2442,#1625,.T.);
#2885=EDGE_CURVE('',#2432,#2442,#1626,.T.);
#2886=EDGE_CURVE('',#2442,#2441,#1627,.T.);
#2887=EDGE_CURVE('',#2443,#2443,#1393,.T.);
#2888=EDGE_CURVE('',#2443,#2444,#1628,.T.);
#2889=EDGE_CURVE('',#2444,#2444,#1394,.T.);
#2890=EDGE_CURVE('',#2445,#2445,#1395,.T.);
#2891=EDGE_CURVE('',#2445,#2446,#1629,.T.);
#2892=EDGE_CURVE('',#2446,#2446,#1396,.T.);
#2893=EDGE_CURVE('',#2426,#2447,#1630,.T.);
#2894=EDGE_CURVE('',#2447,#2448,#1631,.T.);
#2895=EDGE_CURVE('',#2448,#2427,#1632,.T.);
#2896=EDGE_CURVE('',#2449,#2425,#1633,.T.);
#2897=EDGE_CURVE('',#2447,#2449,#1634,.T.);
#2898=EDGE_CURVE('',#2448,#2450,#1635,.T.);
#2899=EDGE_CURVE('',#2428,#2450,#1636,.T.);
#2900=EDGE_CURVE('',#2450,#2449,#1637,.T.);
#2901=EDGE_CURVE('',#2422,#2451,#1638,.T.);
#2902=EDGE_CURVE('',#2451,#2452,#1639,.T.);
#2903=EDGE_CURVE('',#2452,#2423,#1640,.T.);
#2904=EDGE_CURVE('',#2453,#2421,#1641,.T.);
#2905=EDGE_CURVE('',#2451,#2453,#1642,.T.);
#2906=EDGE_CURVE('',#2452,#2454,#1643,.T.);
#2907=EDGE_CURVE('',#2424,#2454,#1644,.T.);
#2908=EDGE_CURVE('',#2454,#2453,#1645,.T.);
#2909=EDGE_CURVE('',#2455,#2410,#1646,.T.);
#2910=EDGE_CURVE('',#2455,#2420,#1647,.T.);
#2911=EDGE_CURVE('',#2456,#2455,#1648,.T.);
#2912=EDGE_CURVE('',#2456,#2419,#1649,.T.);
#2913=EDGE_CURVE('',#2411,#2456,#1650,.T.);
#2914=EDGE_CURVE('',#2457,#2458,#1651,.T.);
#2915=EDGE_CURVE('',#2459,#2457,#1397,.T.);
#2916=EDGE_CURVE('',#2460,#2459,#1652,.T.);
#2917=EDGE_CURVE('',#2460,#2458,#1398,.T.);
#2918=EDGE_CURVE('',#2459,#2457,#1653,.T.);
#2919=EDGE_CURVE('',#2461,#2460,#1654,.T.);
#2920=EDGE_CURVE('',#2462,#2461,#1655,.T.);
#2921=EDGE_CURVE('',#2463,#2462,#1656,.T.);
#2922=EDGE_CURVE('',#2464,#2463,#1657,.T.);
#2923=EDGE_CURVE('',#2458,#2464,#1658,.T.);
#2924=EDGE_CURVE('',#2465,#2465,#1399,.T.);
#2925=EDGE_CURVE('',#2466,#2466,#1400,.T.);
#2926=EDGE_CURVE('',#2466,#2467,#1659,.T.);
#2927=EDGE_CURVE('',#2467,#2467,#1401,.T.);
#2928=EDGE_CURVE('',#2465,#2468,#1660,.T.);
#2929=EDGE_CURVE('',#2468,#2468,#1402,.T.);
#2930=EDGE_CURVE('',#2464,#2469,#1661,.T.);
#2931=EDGE_CURVE('',#2469,#2470,#1662,.T.);
#2932=EDGE_CURVE('',#2470,#2461,#1663,.T.);
#2933=EDGE_CURVE('',#2471,#2471,#1403,.T.);
#2934=EDGE_CURVE('',#2471,#2472,#1664,.T.);
#2935=EDGE_CURVE('',#2472,#2472,#1404,.T.);
#2936=EDGE_CURVE('',#2469,#2473,#1665,.T.);
#2937=EDGE_CURVE('',#2474,#2473,#1666,.T.);
#2938=EDGE_CURVE('',#2470,#2474,#1667,.T.);
#2939=EDGE_CURVE('',#2475,#2476,#1668,.T.);
#2940=EDGE_CURVE('',#2475,#2477,#1669,.T.);
#2941=EDGE_CURVE('',#2478,#2477,#1670,.T.);
#2942=EDGE_CURVE('',#2476,#2478,#1671,.T.);
#2943=EDGE_CURVE('',#2477,#2474,#1672,.T.);
#2944=EDGE_CURVE('',#2473,#2478,#1673,.T.);
#2945=EDGE_CURVE('',#2476,#2479,#1674,.T.);
#2946=EDGE_CURVE('',#2479,#2480,#1675,.T.);
#2947=EDGE_CURVE('',#2480,#2475,#1676,.T.);
#2948=EDGE_CURVE('',#2481,#2481,#1405,.T.);
#2949=EDGE_CURVE('',#2481,#2482,#1677,.T.);
#2950=EDGE_CURVE('',#2482,#2482,#1406,.T.);
#2951=EDGE_CURVE('',#2479,#2483,#1678,.T.);
#2952=EDGE_CURVE('',#2484,#2483,#1679,.T.);
#2953=EDGE_CURVE('',#2480,#2484,#1680,.T.);
#2954=EDGE_CURVE('',#2485,#2486,#1681,.T.);
#2955=EDGE_CURVE('',#2485,#2487,#1682,.T.);
#2956=EDGE_CURVE('',#2488,#2487,#1683,.T.);
#2957=EDGE_CURVE('',#2486,#2488,#1684,.T.);
#2958=EDGE_CURVE('',#2487,#2484,#1685,.T.);
#2959=EDGE_CURVE('',#2483,#2488,#1686,.T.);
#2960=EDGE_CURVE('',#2486,#2489,#1687,.T.);
#2961=EDGE_CURVE('',#2489,#2490,#1688,.T.);
#2962=EDGE_CURVE('',#2490,#2485,#1689,.T.);
#2963=EDGE_CURVE('',#2462,#2491,#1690,.T.);
#2964=EDGE_CURVE('',#2492,#2491,#1691,.T.);
#2965=EDGE_CURVE('',#2463,#2492,#1692,.T.);
#2966=EDGE_CURVE('',#2491,#2493,#1693,.T.);
#2967=EDGE_CURVE('',#2493,#2494,#1694,.T.);
#2968=EDGE_CURVE('',#2494,#2492,#1695,.T.);
#2969=EDGE_CURVE('',#2495,#2494,#1696,.T.);
#2970=EDGE_CURVE('',#2495,#2489,#1697,.T.);
#2971=EDGE_CURVE('',#2496,#2493,#1698,.T.);
#2972=EDGE_CURVE('',#2496,#2490,#1699,.T.);
#2973=EDGE_CURVE('',#2495,#2496,#1700,.T.);
#2974=EDGE_CURVE('',#2497,#2497,#1407,.T.);
#2975=EDGE_CURVE('',#2497,#2498,#1701,.T.);
#2976=EDGE_CURVE('',#2498,#2498,#1408,.T.);
#2977=EDGE_CURVE('',#2498,#2499,#1702,.T.);
#2978=EDGE_CURVE('',#2499,#2499,#1409,.T.);
#2979=EDGE_CURVE('',#2500,#2500,#1410,.T.);
#2980=EDGE_CURVE('',#2500,#2501,#1703,.T.);
#2981=EDGE_CURVE('',#2501,#2501,#1411,.T.);
#2982=EDGE_CURVE('',#2502,#2503,#1704,.T.);
#2983=EDGE_CURVE('',#2503,#2504,#1705,.T.);
#2984=EDGE_CURVE('',#2504,#2505,#1706,.T.);
#2985=EDGE_CURVE('',#2502,#2505,#1707,.T.);
#2986=EDGE_CURVE('',#2503,#2506,#1708,.T.);
#2987=EDGE_CURVE('',#2506,#2507,#1709,.T.);
#2988=EDGE_CURVE('',#2507,#2504,#1710,.T.);
#2989=EDGE_CURVE('',#2506,#2508,#1711,.T.);
#2990=EDGE_CURVE('',#2508,#2509,#1712,.T.);
#2991=EDGE_CURVE('',#2509,#2507,#1713,.T.);
#2992=EDGE_CURVE('',#2508,#2510,#1714,.T.);
#2993=EDGE_CURVE('',#2510,#2511,#1715,.T.);
#2994=EDGE_CURVE('',#2511,#2509,#1716,.T.);
#2995=EDGE_CURVE('',#2510,#2512,#1717,.T.);
#2996=EDGE_CURVE('',#2512,#2513,#1718,.T.);
#2997=EDGE_CURVE('',#2513,#2511,#1719,.T.);
#2998=EDGE_CURVE('',#2512,#2502,#1720,.T.);
#2999=EDGE_CURVE('',#2505,#2513,#1721,.T.);
#3000=EDGE_CURVE('',#2514,#2514,#1412,.T.);
#3001=EDGE_CURVE('',#2515,#2515,#1413,.T.);
#3002=EDGE_CURVE('',#2516,#2516,#1414,.T.);
#3003=EDGE_CURVE('',#2516,#2515,#1722,.T.);
#3004=EDGE_CURVE('',#2517,#2517,#1415,.T.);
#3005=EDGE_CURVE('',#2517,#2516,#1723,.T.);
#3006=EDGE_CURVE('',#2518,#2518,#1416,.T.);
#3007=EDGE_CURVE('',#2518,#2517,#1724,.T.);
#3008=EDGE_CURVE('',#2519,#2519,#1417,.T.);
#3009=EDGE_CURVE('',#2520,#2520,#1418,.F.);
#3010=EDGE_CURVE('',#2520,#2519,#1725,.T.);
#3011=EDGE_CURVE('',#2514,#2520,#1726,.T.);
#3012=EDGE_CURVE('',#2521,#2521,#1419,.T.);
#3013=EDGE_CURVE('',#2521,#2522,#1727,.T.);
#3014=EDGE_CURVE('',#2522,#2522,#1420,.T.);
#3015=EDGE_CURVE('',#2523,#2523,#1421,.T.);
#3016=EDGE_CURVE('',#2523,#2524,#1728,.T.);
#3017=EDGE_CURVE('',#2524,#2524,#1422,.T.);
#3018=EDGE_CURVE('',#2525,#2525,#1423,.T.);
#3019=EDGE_CURVE('',#2525,#2526,#1729,.T.);
#3020=EDGE_CURVE('',#2526,#2526,#1424,.T.);
#3021=EDGE_CURVE('',#2527,#2527,#1425,.T.);
#3022=EDGE_CURVE('',#2527,#2528,#1730,.T.);
#3023=EDGE_CURVE('',#2528,#2528,#1426,.T.);
#3024=EDGE_CURVE('',#2529,#2529,#1427,.T.);
#3025=EDGE_CURVE('',#2529,#2530,#1731,.T.);
#3026=EDGE_CURVE('',#2530,#2530,#1428,.T.);
#3027=EDGE_CURVE('',#2531,#2531,#1429,.T.);
#3028=EDGE_CURVE('',#2531,#2532,#1732,.T.);
#3029=EDGE_CURVE('',#2532,#2532,#1430,.T.);
#3030=EDGE_CURVE('',#2533,#2533,#1431,.T.);
#3031=EDGE_CURVE('',#2533,#2534,#1733,.T.);
#3032=EDGE_CURVE('',#2534,#2534,#1432,.T.);
#3033=EDGE_CURVE('',#2535,#2535,#1433,.T.);
#3034=EDGE_CURVE('',#2535,#2536,#1734,.T.);
#3035=EDGE_CURVE('',#2536,#2536,#1434,.T.);
#3036=EDGE_CURVE('',#2537,#2537,#1435,.T.);
#3037=EDGE_CURVE('',#2537,#2538,#1735,.T.);
#3038=EDGE_CURVE('',#2538,#2538,#1436,.T.);
#3039=EDGE_CURVE('',#2539,#2539,#1437,.T.);
#3040=EDGE_CURVE('',#2539,#2540,#1736,.T.);
#3041=EDGE_CURVE('',#2540,#2540,#1438,.T.);
#3042=EDGE_CURVE('',#2541,#2541,#1439,.T.);
#3043=EDGE_CURVE('',#2541,#2542,#1737,.T.);
#3044=EDGE_CURVE('',#2542,#2542,#1440,.T.);
#3045=EDGE_CURVE('',#2543,#2543,#1441,.T.);
#3046=EDGE_CURVE('',#2543,#2544,#1738,.T.);
#3047=EDGE_CURVE('',#2544,#2544,#1442,.T.);
#3048=EDGE_CURVE('',#2545,#2545,#1443,.T.);
#3049=EDGE_CURVE('',#2545,#2546,#1739,.T.);
#3050=EDGE_CURVE('',#2546,#2546,#1444,.T.);
#3051=EDGE_CURVE('',#2547,#2547,#1445,.T.);
#3052=EDGE_CURVE('',#2547,#2548,#1740,.T.);
#3053=EDGE_CURVE('',#2548,#2548,#1446,.T.);
#3054=EDGE_CURVE('',#2549,#2549,#1447,.T.);
#3055=EDGE_CURVE('',#2549,#2550,#1741,.T.);
#3056=EDGE_CURVE('',#2550,#2550,#1448,.T.);
#3057=EDGE_CURVE('',#2551,#2551,#1449,.T.);
#3058=EDGE_CURVE('',#2551,#2552,#1742,.T.);
#3059=EDGE_CURVE('',#2552,#2552,#1450,.T.);
#3060=EDGE_CURVE('',#2553,#2553,#1451,.T.);
#3061=EDGE_CURVE('',#2553,#2554,#1743,.T.);
#3062=EDGE_CURVE('',#2554,#2554,#1452,.T.);
#3063=EDGE_CURVE('',#2555,#2555,#1453,.T.);
#3064=EDGE_CURVE('',#2555,#2556,#1744,.T.);
#3065=EDGE_CURVE('',#2556,#2556,#1454,.T.);
#3066=EDGE_CURVE('',#2557,#2557,#1455,.T.);
#3067=EDGE_CURVE('',#2557,#2558,#1745,.T.);
#3068=EDGE_CURVE('',#2558,#2558,#1456,.T.);
#3069=EDGE_CURVE('',#2559,#2559,#1457,.T.);
#3070=EDGE_CURVE('',#2559,#2560,#1746,.T.);
#3071=EDGE_CURVE('',#2560,#2560,#1458,.T.);
#3072=EDGE_CURVE('',#2561,#2561,#1459,.T.);
#3073=EDGE_CURVE('',#2561,#2562,#1747,.T.);
#3074=EDGE_CURVE('',#2562,#2562,#1460,.T.);
#3075=EDGE_CURVE('',#2563,#2563,#1461,.T.);
#3076=EDGE_CURVE('',#2563,#2564,#1748,.T.);
#3077=EDGE_CURVE('',#2564,#2564,#1462,.T.);
#3078=EDGE_CURVE('',#2565,#2565,#1463,.T.);
#3079=EDGE_CURVE('',#2565,#2566,#1749,.T.);
#3080=EDGE_CURVE('',#2566,#2566,#1464,.T.);
#3081=EDGE_CURVE('',#2567,#2567,#1465,.T.);
#3082=EDGE_CURVE('',#2567,#2568,#1750,.T.);
#3083=EDGE_CURVE('',#2568,#2568,#1466,.T.);
#3084=EDGE_CURVE('',#2569,#2569,#1467,.T.);
#3085=EDGE_CURVE('',#2569,#2570,#1751,.T.);
#3086=EDGE_CURVE('',#2570,#2570,#1468,.T.);
#3087=EDGE_CURVE('',#2571,#2571,#1469,.T.);
#3088=EDGE_CURVE('',#2571,#2572,#1752,.T.);
#3089=EDGE_CURVE('',#2572,#2572,#1470,.T.);
#3090=EDGE_CURVE('',#2573,#2573,#1471,.T.);
#3091=EDGE_CURVE('',#2573,#2574,#1753,.T.);
#3092=EDGE_CURVE('',#2574,#2574,#1472,.T.);
#3093=EDGE_CURVE('',#2575,#2575,#1473,.T.);
#3094=EDGE_CURVE('',#2575,#2576,#1754,.T.);
#3095=EDGE_CURVE('',#2576,#2576,#1474,.T.);
#3096=EDGE_CURVE('',#2577,#2578,#1755,.T.);
#3097=EDGE_CURVE('',#2578,#2579,#1756,.T.);
#3098=EDGE_CURVE('',#2580,#2579,#1757,.T.);
#3099=EDGE_CURVE('',#2577,#2580,#1758,.T.);
#3100=EDGE_CURVE('',#2581,#2577,#1759,.T.);
#3101=EDGE_CURVE('',#2582,#2580,#1760,.T.);
#3102=EDGE_CURVE('',#2581,#2582,#1761,.T.);
#3103=EDGE_CURVE('',#2583,#2581,#1762,.T.);
#3104=EDGE_CURVE('',#2584,#2582,#1763,.T.);
#3105=EDGE_CURVE('',#2583,#2584,#1764,.T.);
#3106=EDGE_CURVE('',#2578,#2583,#1765,.T.);
#3107=EDGE_CURVE('',#2579,#2584,#1766,.T.);
#3108=EDGE_CURVE('',#2585,#2585,#1475,.T.);
#3109=EDGE_CURVE('',#2585,#2586,#1767,.T.);
#3110=EDGE_CURVE('',#2586,#2586,#1476,.T.);
#3111=EDGE_CURVE('',#2587,#2587,#1477,.T.);
#3112=EDGE_CURVE('',#2587,#2588,#1768,.T.);
#3113=EDGE_CURVE('',#2588,#2588,#1478,.T.);
#3114=EDGE_CURVE('',#2589,#2590,#1769,.T.);
#3115=EDGE_CURVE('',#2590,#2591,#1770,.T.);
#3116=EDGE_CURVE('',#2592,#2591,#1771,.T.);
#3117=EDGE_CURVE('',#2589,#2592,#1772,.T.);
#3118=EDGE_CURVE('',#2593,#2589,#1773,.T.);
#3119=EDGE_CURVE('',#2594,#2592,#1774,.T.);
#3120=EDGE_CURVE('',#2593,#2594,#1775,.T.);
#3121=EDGE_CURVE('',#2595,#2593,#1776,.T.);
#3122=EDGE_CURVE('',#2596,#2594,#1777,.T.);
#3123=EDGE_CURVE('',#2595,#2596,#1778,.T.);
#3124=EDGE_CURVE('',#2590,#2595,#1779,.T.);
#3125=EDGE_CURVE('',#2591,#2596,#1780,.T.);
#3126=EDGE_CURVE('',#2597,#2597,#1479,.F.);
#3127=EDGE_CURVE('',#2597,#2598,#1781,.T.);
#3128=EDGE_CURVE('',#2598,#2598,#1480,.F.);
#3129=EDGE_CURVE('',#2599,#2599,#1481,.T.);
#3130=EDGE_CURVE('',#2599,#2597,#1782,.T.);
#3131=EDGE_CURVE('',#2600,#2600,#1482,.T.);
#3132=EDGE_CURVE('',#2600,#2601,#1783,.T.);
#3133=EDGE_CURVE('',#2602,#2601,#204,.T.);
#3134=EDGE_CURVE('',#2603,#2602,#205,.T.);
#3135=EDGE_CURVE('',#2604,#2603,#206,.T.);
#3136=EDGE_CURVE('',#2605,#2604,#207,.T.);
#3137=EDGE_CURVE('',#2606,#2605,#208,.T.);
#3138=EDGE_CURVE('',#2601,#2606,#209,.T.);
#3139=EDGE_CURVE('',#2607,#2605,#1784,.T.);
#3140=EDGE_CURVE('',#2607,#2608,#1785,.T.);
#3141=EDGE_CURVE('',#2608,#2606,#1786,.T.);
#3142=EDGE_CURVE('',#2609,#2604,#1787,.T.);
#3143=EDGE_CURVE('',#2609,#2607,#1788,.T.);
#3144=EDGE_CURVE('',#2610,#2603,#1789,.T.);
#3145=EDGE_CURVE('',#2610,#2609,#1790,.T.);
#3146=EDGE_CURVE('',#2611,#2602,#1791,.T.);
#3147=EDGE_CURVE('',#2611,#2610,#1792,.T.);
#3148=EDGE_CURVE('',#2612,#2601,#1793,.T.);
#3149=EDGE_CURVE('',#2612,#2611,#1794,.T.);
#3150=EDGE_CURVE('',#2608,#2612,#1795,.T.);
#3151=EDGE_CURVE('',#2613,#2614,#210,.T.);
#3152=EDGE_CURVE('',#2615,#2613,#211,.T.);
#3153=EDGE_CURVE('',#2615,#2616,#1796,.T.);
#3154=EDGE_CURVE('',#2616,#2616,#1483,.T.);
#3155=EDGE_CURVE('',#2617,#2615,#212,.T.);
#3156=EDGE_CURVE('',#2618,#2617,#213,.T.);
#3157=EDGE_CURVE('',#2619,#2618,#214,.T.);
#3158=EDGE_CURVE('',#2614,#2619,#215,.T.);
#3159=EDGE_CURVE('',#2620,#2620,#1484,.T.);
#3160=EDGE_CURVE('',#2620,#2621,#1797,.T.);
#3161=EDGE_CURVE('',#2622,#2621,#216,.T.);
#3162=EDGE_CURVE('',#2623,#2622,#217,.T.);
#3163=EDGE_CURVE('',#2624,#2623,#218,.T.);
#3164=EDGE_CURVE('',#2625,#2624,#219,.T.);
#3165=EDGE_CURVE('',#2626,#2625,#220,.T.);
#3166=EDGE_CURVE('',#2621,#2626,#221,.T.);
#3167=EDGE_CURVE('',#2617,#2626,#1798,.T.);
#3168=EDGE_CURVE('',#2618,#2625,#1799,.T.);
#3169=EDGE_CURVE('',#2615,#2621,#1800,.T.);
#3170=EDGE_CURVE('',#2613,#2622,#1801,.T.);
#3171=EDGE_CURVE('',#2627,#2627,#1485,.F.);
#3172=EDGE_CURVE('',#2627,#2628,#1802,.T.);
#3173=EDGE_CURVE('',#2628,#2628,#1486,.F.);
#3174=EDGE_CURVE('',#2614,#2623,#1803,.T.);
#3175=EDGE_CURVE('',#2619,#2624,#1804,.T.);
#3176=EDGE_CURVE('',#2629,#2629,#1487,.T.);
#3177=EDGE_CURVE('',#2629,#2630,#1805,.T.);
#3178=EDGE_CURVE('',#2630,#2630,#1488,.T.);
#3179=EDGE_CURVE('',#2631,#2631,#1489,.T.);
#3180=EDGE_CURVE('',#2631,#2632,#1806,.T.);
#3181=EDGE_CURVE('',#2632,#2632,#1490,.T.);
#3182=EDGE_CURVE('',#2633,#2633,#1491,.T.);
#3183=EDGE_CURVE('',#2634,#2634,#1492,.T.);
#3184=EDGE_CURVE('',#2634,#2633,#1807,.T.);
#3185=EDGE_CURVE('',#2635,#2635,#1493,.T.);
#3186=EDGE_CURVE('',#2635,#2634,#1808,.T.);
#3187=EDGE_CURVE('',#2636,#2637,#1494,.T.);
#3188=EDGE_CURVE('',#2637,#2636,#1809,.T.);
#3189=EDGE_CURVE('',#2638,#2636,#1810,.T.);
#3190=EDGE_CURVE('',#2639,#2638,#222,.T.);
#3191=EDGE_CURVE('',#2640,#2639,#1811,.T.);
#3192=EDGE_CURVE('',#2641,#2640,#223,.T.);
#3193=EDGE_CURVE('',#2637,#2641,#1812,.T.);
#3194=EDGE_CURVE('',#2642,#2641,#1495,.T.);
#3195=EDGE_CURVE('',#2642,#2643,#1813,.T.);
#3196=EDGE_CURVE('',#2643,#2644,#1496,.T.);
#3197=EDGE_CURVE('',#2644,#2645,#1814,.T.);
#3198=EDGE_CURVE('',#2645,#2645,#1497,.T.);
#3199=EDGE_CURVE('',#2644,#2646,#1498,.T.);
#3200=EDGE_CURVE('',#2646,#2647,#1815,.T.);
#3201=EDGE_CURVE('',#2638,#2647,#1499,.T.);
#3202=EDGE_CURVE('',#2648,#2640,#1500,.T.);
#3203=EDGE_CURVE('',#2648,#2642,#224,.T.);
#3204=EDGE_CURVE('',#2643,#2646,#1816,.T.);
#3205=EDGE_CURVE('',#2649,#2648,#1817,.T.);
#3206=EDGE_CURVE('',#2647,#2649,#225,.T.);
#3207=EDGE_CURVE('',#2639,#2649,#1501,.T.);
#3208=EDGE_CURVE('',#2650,#2651,#1818,.T.);
#3209=EDGE_CURVE('',#2651,#2652,#1819,.T.);
#3210=EDGE_CURVE('',#2652,#2653,#1820,.T.);
#3211=EDGE_CURVE('',#2650,#2653,#1821,.T.);
#3212=EDGE_CURVE('',#2651,#2654,#1822,.T.);
#3213=EDGE_CURVE('',#2654,#2655,#1823,.T.);
#3214=EDGE_CURVE('',#2655,#2652,#1824,.T.);
#3215=EDGE_CURVE('',#2654,#2656,#1825,.T.);
#3216=EDGE_CURVE('',#2656,#2657,#1826,.T.);
#3217=EDGE_CURVE('',#2657,#2655,#1827,.T.);
#3218=EDGE_CURVE('',#2656,#2658,#1828,.T.);
#3219=EDGE_CURVE('',#2658,#2659,#1829,.T.);
#3220=EDGE_CURVE('',#2659,#2657,#1830,.T.);
#3221=EDGE_CURVE('',#2658,#2660,#1831,.T.);
#3222=EDGE_CURVE('',#2660,#2661,#1832,.T.);
#3223=EDGE_CURVE('',#2661,#2659,#1833,.T.);
#3224=EDGE_CURVE('',#2660,#2650,#1834,.T.);
#3225=EDGE_CURVE('',#2653,#2661,#1835,.T.);
#3226=EDGE_CURVE('',#2662,#2662,#1502,.T.);
#3227=EDGE_CURVE('',#2663,#2663,#1503,.T.);
#3228=EDGE_CURVE('',#2664,#2664,#1504,.T.);
#3229=EDGE_CURVE('',#2664,#2663,#1836,.T.);
#3230=EDGE_CURVE('',#2665,#2665,#1505,.T.);
#3231=EDGE_CURVE('',#2665,#2664,#1837,.T.);
#3232=EDGE_CURVE('',#2666,#2666,#1506,.T.);
#3233=EDGE_CURVE('',#2666,#2665,#1838,.T.);
#3234=EDGE_CURVE('',#2667,#2667,#1507,.T.);
#3235=EDGE_CURVE('',#2668,#2668,#1508,.F.);
#3236=EDGE_CURVE('',#2668,#2667,#1839,.T.);
#3237=EDGE_CURVE('',#2662,#2668,#1840,.T.);
#3238=EDGE_CURVE('',#2669,#2669,#1509,.T.);
#3239=EDGE_CURVE('',#2669,#2670,#1841,.T.);
#3240=EDGE_CURVE('',#2670,#2670,#1510,.T.);
#3241=EDGE_CURVE('',#2671,#2671,#1511,.T.);
#3242=EDGE_CURVE('',#2671,#2672,#1842,.T.);
#3243=EDGE_CURVE('',#2672,#2672,#1512,.T.);
#3244=EDGE_CURVE('',#2673,#2674,#1843,.T.);
#3245=EDGE_CURVE('',#2675,#2673,#1513,.T.);
#3246=EDGE_CURVE('',#2676,#2675,#1844,.T.);
#3247=EDGE_CURVE('',#2676,#2674,#1514,.T.);
#3248=EDGE_CURVE('',#2677,#2676,#1845,.T.);
#3249=EDGE_CURVE('',#2678,#2677,#1515,.T.);
#3250=EDGE_CURVE('',#2674,#2678,#1846,.T.);
#3251=EDGE_CURVE('',#2679,#2675,#1847,.T.);
#3252=EDGE_CURVE('',#2677,#2679,#1848,.T.);
#3253=EDGE_CURVE('',#2673,#2680,#1849,.T.);
#3254=EDGE_CURVE('',#2679,#2680,#1516,.T.);
#3255=EDGE_CURVE('',#2680,#2678,#1850,.T.);
#3256=EDGE_CURVE('',#2681,#2681,#1517,.T.);
#3257=EDGE_CURVE('',#2681,#2682,#1851,.T.);
#3258=EDGE_CURVE('',#2682,#2682,#1518,.T.);
#3259=EDGE_CURVE('',#2683,#2683,#1519,.T.);
#3260=EDGE_CURVE('',#2683,#2684,#1852,.T.);
#3261=EDGE_CURVE('',#2684,#2684,#1520,.T.);
#3262=EDGE_CURVE('',#2685,#2686,#1853,.T.);
#3263=EDGE_CURVE('',#2685,#2687,#1854,.T.);
#3264=EDGE_CURVE('',#2688,#2687,#1855,.T.);
#3265=EDGE_CURVE('',#2686,#2688,#1856,.T.);
#3266=EDGE_CURVE('',#2689,#2690,#1857,.T.);
#3267=EDGE_CURVE('',#2690,#2691,#1858,.T.);
#3268=EDGE_CURVE('',#2691,#2692,#1859,.T.);
#3269=EDGE_CURVE('',#2692,#2689,#1860,.T.);
#3270=EDGE_CURVE('',#2693,#2694,#1861,.T.);
#3271=EDGE_CURVE('',#2693,#2691,#1862,.T.);
#3272=EDGE_CURVE('',#2694,#2690,#1863,.T.);
#3273=EDGE_CURVE('',#2687,#2693,#1864,.T.);
#3274=EDGE_CURVE('',#2694,#2688,#1865,.T.);
#3275=EDGE_CURVE('',#2695,#2696,#1866,.T.);
#3276=EDGE_CURVE('',#2697,#2696,#1867,.T.);
#3277=EDGE_CURVE('',#2698,#2697,#1521,.T.);
#3278=EDGE_CURVE('',#2695,#2698,#1868,.T.);
#3279=EDGE_CURVE('',#2696,#2699,#1869,.T.);
#3280=EDGE_CURVE('',#2700,#2699,#1870,.T.);
#3281=EDGE_CURVE('',#2697,#2700,#1871,.T.);
#3282=EDGE_CURVE('',#2699,#2701,#1872,.T.);
#3283=EDGE_CURVE('',#2701,#2702,#1873,.T.);
#3284=EDGE_CURVE('',#2700,#2702,#1522,.T.);
#3285=EDGE_CURVE('',#2701,#2695,#1874,.T.);
#3286=EDGE_CURVE('',#2702,#2698,#1875,.T.);
#3287=EDGE_CURVE('',#2703,#2703,#1523,.T.);
#3288=EDGE_CURVE('',#2703,#2704,#1876,.T.);
#3289=EDGE_CURVE('',#2704,#2704,#1524,.T.);
#3290=EDGE_CURVE('',#2705,#2685,#1877,.T.);
#3291=EDGE_CURVE('',#2706,#2705,#1878,.T.);
#3292=EDGE_CURVE('',#2707,#2706,#1879,.T.);
#3293=EDGE_CURVE('',#2707,#2692,#1880,.T.);
#3294=EDGE_CURVE('',#2686,#2708,#1881,.T.);
#3295=EDGE_CURVE('',#2708,#2705,#1882,.T.);
#3296=EDGE_CURVE('',#2709,#2707,#1883,.T.);
#3297=EDGE_CURVE('',#2709,#2689,#1884,.T.);
#3298=EDGE_CURVE('',#2706,#2710,#1885,.T.);
#3299=EDGE_CURVE('',#2710,#2708,#1886,.T.);
#3300=EDGE_CURVE('',#2710,#2709,#1887,.T.);
#3301=EDGE_CURVE('',#2711,#2711,#1525,.T.);
#3302=EDGE_CURVE('',#2711,#2712,#1888,.T.);
#3303=EDGE_CURVE('',#2712,#2712,#1526,.T.);
#3304=EDGE_CURVE('',#2713,#2713,#1527,.T.);
#3305=EDGE_CURVE('',#2713,#2714,#1889,.T.);
#3306=EDGE_CURVE('',#2714,#2714,#1528,.T.);
#3307=EDGE_CURVE('',#2715,#2716,#1890,.T.);
#3308=EDGE_CURVE('',#2716,#2717,#1891,.T.);
#3309=EDGE_CURVE('',#2717,#2718,#1892,.T.);
#3310=EDGE_CURVE('',#2715,#2718,#1893,.T.);
#3311=EDGE_CURVE('',#2716,#2719,#1894,.T.);
#3312=EDGE_CURVE('',#2719,#2720,#1895,.T.);
#3313=EDGE_CURVE('',#2720,#2717,#1896,.T.);
#3314=EDGE_CURVE('',#2719,#2721,#1897,.T.);
#3315=EDGE_CURVE('',#2721,#2722,#1898,.T.);
#3316=EDGE_CURVE('',#2722,#2720,#1899,.T.);
#3317=EDGE_CURVE('',#2721,#2723,#1900,.T.);
#3318=EDGE_CURVE('',#2723,#2724,#1901,.T.);
#3319=EDGE_CURVE('',#2724,#2722,#1902,.T.);
#3320=EDGE_CURVE('',#2723,#2725,#1903,.T.);
#3321=EDGE_CURVE('',#2725,#2726,#1904,.T.);
#3322=EDGE_CURVE('',#2726,#2724,#1905,.T.);
#3323=EDGE_CURVE('',#2725,#2715,#1906,.T.);
#3324=EDGE_CURVE('',#2718,#2726,#1907,.T.);
#3325=EDGE_CURVE('',#2727,#2727,#1529,.T.);
#3326=EDGE_CURVE('',#2728,#2728,#1530,.T.);
#3327=EDGE_CURVE('',#2729,#2729,#1531,.T.);
#3328=EDGE_CURVE('',#2729,#2728,#1908,.T.);
#3329=EDGE_CURVE('',#2730,#2730,#1532,.T.);
#3330=EDGE_CURVE('',#2730,#2729,#1909,.T.);
#3331=EDGE_CURVE('',#2731,#2731,#1533,.T.);
#3332=EDGE_CURVE('',#2731,#2730,#1910,.T.);
#3333=EDGE_CURVE('',#2732,#2732,#1534,.T.);
#3334=EDGE_CURVE('',#2733,#2733,#1535,.F.);
#3335=EDGE_CURVE('',#2733,#2732,#1911,.T.);
#3336=EDGE_CURVE('',#2727,#2733,#1912,.T.);
#3337=EDGE_CURVE('',#2734,#2734,#1536,.T.);
#3338=EDGE_CURVE('',#2734,#2735,#1913,.T.);
#3339=EDGE_CURVE('',#2735,#2735,#1537,.T.);
#3340=EDGE_CURVE('',#2736,#2736,#1538,.T.);
#3341=EDGE_CURVE('',#2736,#2737,#1914,.T.);
#3342=EDGE_CURVE('',#2737,#2737,#1539,.T.);
#3343=EDGE_CURVE('',#2738,#2739,#1915,.T.);
#3344=EDGE_CURVE('',#2740,#2738,#1540,.T.);
#3345=EDGE_CURVE('',#2741,#2740,#1916,.T.);
#3346=EDGE_CURVE('',#2741,#2739,#1541,.T.);
#3347=EDGE_CURVE('',#2739,#2742,#1917,.T.);
#3348=EDGE_CURVE('',#2743,#2742,#1918,.T.);
#3349=EDGE_CURVE('',#2738,#2743,#1919,.T.);
#3350=EDGE_CURVE('',#2744,#2741,#1920,.T.);
#3351=EDGE_CURVE('',#2742,#2744,#1542,.T.);
#3352=EDGE_CURVE('',#2745,#2740,#1921,.T.);
#3353=EDGE_CURVE('',#2744,#2745,#1922,.T.);
#3354=EDGE_CURVE('',#2743,#2745,#1543,.T.);
#3355=EDGE_CURVE('',#2746,#2746,#1544,.T.);
#3356=EDGE_CURVE('',#2746,#2747,#1923,.T.);
#3357=EDGE_CURVE('',#2747,#2747,#1545,.T.);
#3358=EDGE_CURVE('',#2748,#2748,#1546,.T.);
#3359=EDGE_CURVE('',#2748,#2749,#1924,.T.);
#3360=EDGE_CURVE('',#2749,#2749,#1547,.T.);
#3361=EDGE_CURVE('',#2750,#2750,#1548,.T.);
#3362=EDGE_CURVE('',#2750,#2751,#1925,.T.);
#3363=EDGE_CURVE('',#2751,#2751,#1549,.T.);
#3364=EDGE_CURVE('',#2752,#2753,#1926,.T.);
#3365=EDGE_CURVE('',#2754,#2752,#1927,.T.);
#3366=EDGE_CURVE('',#2755,#2754,#1928,.T.);
#3367=EDGE_CURVE('',#2755,#2753,#1929,.T.);
#3368=EDGE_CURVE('',#2756,#2757,#1930,.T.);
#3369=EDGE_CURVE('',#2757,#2758,#1931,.T.);
#3370=EDGE_CURVE('',#2758,#2759,#1932,.T.);
#3371=EDGE_CURVE('',#2759,#2756,#1933,.T.);
#3372=EDGE_CURVE('',#2760,#2752,#1934,.T.);
#3373=EDGE_CURVE('',#2760,#2757,#1935,.T.);
#3374=EDGE_CURVE('',#2761,#2756,#1936,.T.);
#3375=EDGE_CURVE('',#2762,#2761,#1937,.T.);
#3376=EDGE_CURVE('',#2762,#2763,#1938,.T.);
#3377=EDGE_CURVE('',#2754,#2763,#1939,.T.);
#3378=EDGE_CURVE('',#2764,#2765,#1940,.T.);
#3379=EDGE_CURVE('',#2765,#2762,#1941,.T.);
#3380=EDGE_CURVE('',#2761,#2764,#1942,.T.);
#3381=EDGE_CURVE('',#2766,#2760,#1943,.T.);
#3382=EDGE_CURVE('',#2766,#2758,#1944,.T.);
#3383=EDGE_CURVE('',#2764,#2759,#1945,.T.);
#3384=EDGE_CURVE('',#2767,#2767,#1550,.T.);
#3385=EDGE_CURVE('',#2753,#2766,#1946,.T.);
#3386=EDGE_CURVE('',#2768,#2755,#1947,.T.);
#3387=EDGE_CURVE('',#2765,#2768,#1948,.T.);
#3388=EDGE_CURVE('',#2763,#2768,#1949,.T.);
#3389=EDGE_CURVE('',#2769,#2769,#1551,.T.);
#3390=EDGE_CURVE('',#2769,#2767,#1950,.T.);
#3391=EDGE_CURVE('',#2770,#2770,#1552,.F.);
#3392=EDGE_CURVE('',#2770,#2771,#1951,.T.);
#3393=EDGE_CURVE('',#2771,#2771,#1553,.F.);
#3394=EDGE_CURVE('',#2772,#2772,#1554,.T.);
#3395=EDGE_CURVE('',#2772,#2770,#1952,.T.);
#3396=EDGE_CURVE('',#2773,#2773,#1555,.T.);
#3397=EDGE_CURVE('',#2773,#2774,#1953,.T.);
#3398=EDGE_CURVE('',#2775,#2774,#226,.T.);
#3399=EDGE_CURVE('',#2776,#2775,#227,.T.);
#3400=EDGE_CURVE('',#2777,#2776,#228,.T.);
#3401=EDGE_CURVE('',#2778,#2777,#229,.T.);
#3402=EDGE_CURVE('',#2779,#2778,#230,.T.);
#3403=EDGE_CURVE('',#2774,#2779,#231,.T.);
#3404=EDGE_CURVE('',#2780,#2778,#1954,.T.);
#3405=EDGE_CURVE('',#2780,#2781,#1955,.T.);
#3406=EDGE_CURVE('',#2781,#2779,#1956,.T.);
#3407=EDGE_CURVE('',#2782,#2777,#1957,.T.);
#3408=EDGE_CURVE('',#2782,#2780,#1958,.T.);
#3409=EDGE_CURVE('',#2783,#2776,#1959,.T.);
#3410=EDGE_CURVE('',#2783,#2782,#1960,.T.);
#3411=EDGE_CURVE('',#2784,#2775,#1961,.T.);
#3412=EDGE_CURVE('',#2784,#2783,#1962,.T.);
#3413=EDGE_CURVE('',#2785,#2774,#1963,.T.);
#3414=EDGE_CURVE('',#2785,#2784,#1964,.T.);
#3415=EDGE_CURVE('',#2781,#2785,#1965,.T.);
#3416=EDGE_CURVE('',#2786,#2787,#232,.T.);
#3417=EDGE_CURVE('',#2788,#2786,#233,.T.);
#3418=EDGE_CURVE('',#2788,#2789,#1966,.T.);
#3419=EDGE_CURVE('',#2789,#2789,#1556,.T.);
#3420=EDGE_CURVE('',#2790,#2788,#234,.T.);
#3421=EDGE_CURVE('',#2791,#2790,#235,.T.);
#3422=EDGE_CURVE('',#2792,#2791,#236,.T.);
#3423=EDGE_CURVE('',#2787,#2792,#237,.T.);
#3424=EDGE_CURVE('',#2793,#2793,#1557,.T.);
#3425=EDGE_CURVE('',#2793,#2794,#1967,.T.);
#3426=EDGE_CURVE('',#2795,#2794,#238,.T.);
#3427=EDGE_CURVE('',#2796,#2795,#239,.T.);
#3428=EDGE_CURVE('',#2797,#2796,#240,.T.);
#3429=EDGE_CURVE('',#2798,#2797,#241,.T.);
#3430=EDGE_CURVE('',#2799,#2798,#242,.T.);
#3431=EDGE_CURVE('',#2794,#2799,#243,.T.);
#3432=EDGE_CURVE('',#2790,#2799,#1968,.T.);
#3433=EDGE_CURVE('',#2791,#2798,#1969,.T.);
#3434=EDGE_CURVE('',#2788,#2794,#1970,.T.);
#3435=EDGE_CURVE('',#2786,#2795,#1971,.T.);
#3436=EDGE_CURVE('',#2800,#2800,#1558,.F.);
#3437=EDGE_CURVE('',#2800,#2801,#1972,.T.);
#3438=EDGE_CURVE('',#2801,#2801,#1559,.F.);
#3439=EDGE_CURVE('',#2787,#2796,#1973,.T.);
#3440=EDGE_CURVE('',#2792,#2797,#1974,.T.);
#3441=EDGE_CURVE('',#2802,#2802,#1560,.T.);
#3442=EDGE_CURVE('',#2802,#2803,#1975,.T.);
#3443=EDGE_CURVE('',#2803,#2803,#1561,.T.);
#3444=EDGE_CURVE('',#2804,#2805,#12,.T.);
#3445=EDGE_CURVE('',#2804,#2806,#1976,.T.);
#3446=EDGE_CURVE('',#2806,#2806,#13,.T.);
#3447=EDGE_CURVE('',#2807,#2804,#14,.T.);
#3448=EDGE_CURVE('',#2805,#2807,#15,.T.);
#3449=EDGE_CURVE('',#2808,#2808,#1562,.T.);
#3450=EDGE_CURVE('',#2809,#2809,#1563,.T.);
#3451=EDGE_CURVE('',#2809,#2808,#1977,.T.);
#3452=EDGE_CURVE('',#2810,#2810,#1564,.T.);
#3453=EDGE_CURVE('',#2810,#2809,#1978,.T.);
#3454=EDGE_CURVE('',#2811,#2811,#1565,.T.);
#3455=EDGE_CURVE('',#2812,#2812,#1566,.T.);
#3456=EDGE_CURVE('',#2812,#2805,#1979,.T.);
#3457=EDGE_CURVE('',#2807,#2811,#1980,.T.);
#3458=EDGE_CURVE('',#2813,#2813,#1567,.T.);
#3459=EDGE_CURVE('',#2813,#2812,#1981,.T.);
#3460=EDGE_CURVE('',#2814,#2814,#1568,.T.);
#3461=EDGE_CURVE('',#2814,#2815,#1982,.T.);
#3462=EDGE_CURVE('',#2815,#2815,#1569,.T.);
#3463=EDGE_CURVE('',#2816,#2816,#1570,.T.);
#3464=EDGE_CURVE('',#2816,#2817,#1983,.T.);
#3465=EDGE_CURVE('',#2817,#2817,#1571,.T.);
#3466=EDGE_CURVE('',#2818,#2818,#1572,.T.);
#3467=EDGE_CURVE('',#2818,#2819,#1984,.T.);
#3468=EDGE_CURVE('',#2819,#2819,#1573,.T.);
#3469=EDGE_CURVE('',#2820,#2820,#1574,.T.);
#3470=EDGE_CURVE('',#2820,#2821,#1985,.T.);
#3471=EDGE_CURVE('',#2821,#2821,#1575,.T.);
#3472=EDGE_CURVE('',#2822,#2822,#1576,.T.);
#3473=EDGE_CURVE('',#2822,#2822,#1577,.T.);
#3474=EDGE_CURVE('',#2823,#2824,#16,.T.);
#3475=EDGE_CURVE('',#2824,#2823,#17,.T.);
#3476=EDGE_CURVE('',#2825,#2826,#1578,.T.);
#3477=EDGE_CURVE('',#2825,#2826,#1986,.T.);
#3478=EDGE_CURVE('',#2826,#2827,#1987,.T.);
#3479=EDGE_CURVE('',#2828,#2827,#1988,.T.);
#3480=EDGE_CURVE('',#2825,#2828,#1989,.T.);
#3481=EDGE_CURVE('',#2829,#2828,#1579,.T.);
#3482=EDGE_CURVE('',#2829,#2824,#1990,.T.);
#3483=EDGE_CURVE('',#2827,#2829,#1580,.T.);
#3484=ORIENTED_EDGE('',*,*,#2830,.F.);
#3485=ORIENTED_EDGE('',*,*,#2831,.F.);
#3486=ORIENTED_EDGE('',*,*,#2832,.T.);
#3487=ORIENTED_EDGE('',*,*,#2833,.F.);
#3488=ORIENTED_EDGE('',*,*,#2834,.T.);
#3489=ORIENTED_EDGE('',*,*,#2835,.T.);
#3490=ORIENTED_EDGE('',*,*,#2834,.F.);
#3491=ORIENTED_EDGE('',*,*,#2836,.F.);
#3492=ORIENTED_EDGE('',*,*,#2835,.F.);
#3493=ORIENTED_EDGE('',*,*,#2837,.T.);
#3494=ORIENTED_EDGE('',*,*,#2838,.T.);
#3495=ORIENTED_EDGE('',*,*,#2839,.F.);
#3496=ORIENTED_EDGE('',*,*,#2840,.F.);
#3497=ORIENTED_EDGE('',*,*,#2841,.T.);
#3498=ORIENTED_EDGE('',*,*,#2842,.T.);
#3499=ORIENTED_EDGE('',*,*,#2843,.F.);
#3500=ORIENTED_EDGE('',*,*,#2844,.T.);
#3501=ORIENTED_EDGE('',*,*,#2845,.T.);
#3502=ORIENTED_EDGE('',*,*,#2836,.T.);
#3503=ORIENTED_EDGE('',*,*,#2833,.T.);
#3504=ORIENTED_EDGE('',*,*,#2846,.F.);
#3505=ORIENTED_EDGE('',*,*,#2847,.F.);
#3506=ORIENTED_EDGE('',*,*,#2830,.T.);
#3507=ORIENTED_EDGE('',*,*,#2845,.F.);
#3508=ORIENTED_EDGE('',*,*,#2848,.F.);
#3509=ORIENTED_EDGE('',*,*,#2849,.T.);
#3510=ORIENTED_EDGE('',*,*,#2837,.F.);
#3511=ORIENTED_EDGE('',*,*,#2832,.F.);
#3512=ORIENTED_EDGE('',*,*,#2850,.F.);
#3513=ORIENTED_EDGE('',*,*,#2851,.F.);
#3514=ORIENTED_EDGE('',*,*,#2838,.F.);
#3515=ORIENTED_EDGE('',*,*,#2849,.F.);
#3516=ORIENTED_EDGE('',*,*,#2846,.T.);
#3517=ORIENTED_EDGE('',*,*,#2844,.F.);
#3518=ORIENTED_EDGE('',*,*,#2852,.F.);
#3519=ORIENTED_EDGE('',*,*,#2853,.F.);
#3520=ORIENTED_EDGE('',*,*,#2831,.T.);
#3521=ORIENTED_EDGE('',*,*,#2847,.T.);
#3522=ORIENTED_EDGE('',*,*,#2853,.T.);
#3523=ORIENTED_EDGE('',*,*,#2854,.F.);
#3524=ORIENTED_EDGE('',*,*,#2850,.T.);
#3525=ORIENTED_EDGE('',*,*,#2848,.T.);
#3526=ORIENTED_EDGE('',*,*,#2851,.T.);
#3527=ORIENTED_EDGE('',*,*,#2854,.T.);
#3528=ORIENTED_EDGE('',*,*,#2852,.T.);
#3529=ORIENTED_EDGE('',*,*,#2843,.T.);
#3530=ORIENTED_EDGE('',*,*,#2855,.T.);
#3531=ORIENTED_EDGE('',*,*,#2856,.T.);
#3532=ORIENTED_EDGE('',*,*,#2857,.T.);
#3533=ORIENTED_EDGE('',*,*,#2839,.T.);
#3534=ORIENTED_EDGE('',*,*,#2858,.T.);
#3535=ORIENTED_EDGE('',*,*,#2859,.T.);
#3536=ORIENTED_EDGE('',*,*,#2860,.T.);
#3537=ORIENTED_EDGE('',*,*,#2861,.T.);
#3538=ORIENTED_EDGE('',*,*,#2862,.T.);
#3539=ORIENTED_EDGE('',*,*,#2863,.T.);
#3540=ORIENTED_EDGE('',*,*,#2864,.T.);
#3541=ORIENTED_EDGE('',*,*,#2865,.T.);
#3542=ORIENTED_EDGE('',*,*,#2866,.T.);
#3543=ORIENTED_EDGE('',*,*,#2867,.T.);
#3544=ORIENTED_EDGE('',*,*,#2868,.T.);
#3545=ORIENTED_EDGE('',*,*,#2869,.T.);
#3546=ORIENTED_EDGE('',*,*,#2870,.T.);
#3547=ORIENTED_EDGE('',*,*,#2871,.T.);
#3548=ORIENTED_EDGE('',*,*,#2872,.F.);
#3549=ORIENTED_EDGE('',*,*,#2873,.T.);
#3550=ORIENTED_EDGE('',*,*,#2871,.F.);
#3551=ORIENTED_EDGE('',*,*,#2873,.F.);
#3552=ORIENTED_EDGE('',*,*,#2874,.F.);
#3553=ORIENTED_EDGE('',*,*,#2875,.T.);
#3554=ORIENTED_EDGE('',*,*,#2870,.F.);
#3555=ORIENTED_EDGE('',*,*,#2875,.F.);
#3556=ORIENTED_EDGE('',*,*,#2876,.F.);
#3557=ORIENTED_EDGE('',*,*,#2877,.T.);
#3558=ORIENTED_EDGE('',*,*,#2878,.F.);
#3559=ORIENTED_EDGE('',*,*,#2877,.F.);
#3560=ORIENTED_EDGE('',*,*,#2867,.F.);
#3561=ORIENTED_EDGE('',*,*,#2879,.T.);
#3562=ORIENTED_EDGE('',*,*,#2880,.T.);
#3563=ORIENTED_EDGE('',*,*,#2881,.T.);
#3564=ORIENTED_EDGE('',*,*,#2866,.F.);
#3565=ORIENTED_EDGE('',*,*,#2882,.F.);
#3566=ORIENTED_EDGE('',*,*,#2883,.F.);
#3567=ORIENTED_EDGE('',*,*,#2879,.F.);
#3568=ORIENTED_EDGE('',*,*,#2878,.T.);
#3569=ORIENTED_EDGE('',*,*,#2868,.F.);
#3570=ORIENTED_EDGE('',*,*,#2881,.F.);
#3571=ORIENTED_EDGE('',*,*,#2884,.T.);
#3572=ORIENTED_EDGE('',*,*,#2885,.F.);
#3573=ORIENTED_EDGE('',*,*,#2876,.T.);
#3574=ORIENTED_EDGE('',*,*,#2880,.F.);
#3575=ORIENTED_EDGE('',*,*,#2883,.T.);
#3576=ORIENTED_EDGE('',*,*,#2886,.F.);
#3577=ORIENTED_EDGE('',*,*,#2884,.F.);
#3578=ORIENTED_EDGE('',*,*,#2869,.F.);
#3579=ORIENTED_EDGE('',*,*,#2885,.T.);
#3580=ORIENTED_EDGE('',*,*,#2886,.T.);
#3581=ORIENTED_EDGE('',*,*,#2882,.T.);
#3582=ORIENTED_EDGE('',*,*,#2887,.F.);
#3583=ORIENTED_EDGE('',*,*,#2888,.T.);
#3584=ORIENTED_EDGE('',*,*,#2889,.F.);
#3585=ORIENTED_EDGE('',*,*,#2888,.F.);
#3586=ORIENTED_EDGE('',*,*,#2890,.F.);
#3587=ORIENTED_EDGE('',*,*,#2891,.T.);
#3588=ORIENTED_EDGE('',*,*,#2892,.F.);
#3589=ORIENTED_EDGE('',*,*,#2891,.F.);
#3590=ORIENTED_EDGE('',*,*,#2863,.F.);
#3591=ORIENTED_EDGE('',*,*,#2893,.T.);
#3592=ORIENTED_EDGE('',*,*,#2894,.T.);
#3593=ORIENTED_EDGE('',*,*,#2895,.T.);
#3594=ORIENTED_EDGE('',*,*,#2890,.T.);
#3595=ORIENTED_EDGE('',*,*,#2862,.F.);
#3596=ORIENTED_EDGE('',*,*,#2896,.F.);
#3597=ORIENTED_EDGE('',*,*,#2897,.F.);
#3598=ORIENTED_EDGE('',*,*,#2893,.F.);
#3599=ORIENTED_EDGE('',*,*,#2864,.F.);
#3600=ORIENTED_EDGE('',*,*,#2895,.F.);
#3601=ORIENTED_EDGE('',*,*,#2898,.T.);
#3602=ORIENTED_EDGE('',*,*,#2899,.F.);
#3603=ORIENTED_EDGE('',*,*,#2894,.F.);
#3604=ORIENTED_EDGE('',*,*,#2897,.T.);
#3605=ORIENTED_EDGE('',*,*,#2900,.F.);
#3606=ORIENTED_EDGE('',*,*,#2898,.F.);
#3607=ORIENTED_EDGE('',*,*,#2865,.F.);
#3608=ORIENTED_EDGE('',*,*,#2899,.T.);
#3609=ORIENTED_EDGE('',*,*,#2900,.T.);
#3610=ORIENTED_EDGE('',*,*,#2896,.T.);
#3611=ORIENTED_EDGE('',*,*,#2892,.T.);
#3612=ORIENTED_EDGE('',*,*,#2859,.F.);
#3613=ORIENTED_EDGE('',*,*,#2901,.T.);
#3614=ORIENTED_EDGE('',*,*,#2902,.T.);
#3615=ORIENTED_EDGE('',*,*,#2903,.T.);
#3616=ORIENTED_EDGE('',*,*,#2887,.T.);
#3617=ORIENTED_EDGE('',*,*,#2858,.F.);
#3618=ORIENTED_EDGE('',*,*,#2904,.F.);
#3619=ORIENTED_EDGE('',*,*,#2905,.F.);
#3620=ORIENTED_EDGE('',*,*,#2901,.F.);
#3621=ORIENTED_EDGE('',*,*,#2860,.F.);
#3622=ORIENTED_EDGE('',*,*,#2903,.F.);
#3623=ORIENTED_EDGE('',*,*,#2906,.T.);
#3624=ORIENTED_EDGE('',*,*,#2907,.F.);
#3625=ORIENTED_EDGE('',*,*,#2902,.F.);
#3626=ORIENTED_EDGE('',*,*,#2905,.T.);
#3627=ORIENTED_EDGE('',*,*,#2908,.F.);
#3628=ORIENTED_EDGE('',*,*,#2906,.F.);
#3629=ORIENTED_EDGE('',*,*,#2861,.F.);
#3630=ORIENTED_EDGE('',*,*,#2907,.T.);
#3631=ORIENTED_EDGE('',*,*,#2908,.T.);
#3632=ORIENTED_EDGE('',*,*,#2904,.T.);
#3633=ORIENTED_EDGE('',*,*,#2889,.T.);
#3634=ORIENTED_EDGE('',*,*,#2909,.T.);
#3635=ORIENTED_EDGE('',*,*,#2840,.T.);
#3636=ORIENTED_EDGE('',*,*,#2857,.F.);
#3637=ORIENTED_EDGE('',*,*,#2910,.F.);
#3638=ORIENTED_EDGE('',*,*,#2911,.T.);
#3639=ORIENTED_EDGE('',*,*,#2910,.T.);
#3640=ORIENTED_EDGE('',*,*,#2856,.F.);
#3641=ORIENTED_EDGE('',*,*,#2912,.F.);
#3642=ORIENTED_EDGE('',*,*,#2913,.T.);
#3643=ORIENTED_EDGE('',*,*,#2912,.T.);
#3644=ORIENTED_EDGE('',*,*,#2855,.F.);
#3645=ORIENTED_EDGE('',*,*,#2842,.F.);
#3646=ORIENTED_EDGE('',*,*,#2913,.F.);
#3647=ORIENTED_EDGE('',*,*,#2841,.F.);
#3648=ORIENTED_EDGE('',*,*,#2909,.F.);
#3649=ORIENTED_EDGE('',*,*,#2911,.F.);
#3650=ORIENTED_EDGE('',*,*,#2872,.T.);
#3651=ORIENTED_EDGE('',*,*,#2874,.T.);
#3652=ORIENTED_EDGE('',*,*,#2914,.F.);
#3653=ORIENTED_EDGE('',*,*,#2915,.F.);
#3654=ORIENTED_EDGE('',*,*,#2916,.F.);
#3655=ORIENTED_EDGE('',*,*,#2917,.T.);
#3656=ORIENTED_EDGE('',*,*,#2918,.F.);
#3657=ORIENTED_EDGE('',*,*,#2915,.T.);
#3658=ORIENTED_EDGE('',*,*,#2919,.F.);
#3659=ORIENTED_EDGE('',*,*,#2920,.F.);
#3660=ORIENTED_EDGE('',*,*,#2921,.F.);
#3661=ORIENTED_EDGE('',*,*,#2922,.F.);
#3662=ORIENTED_EDGE('',*,*,#2923,.F.);
#3663=ORIENTED_EDGE('',*,*,#2917,.F.);
#3664=ORIENTED_EDGE('',*,*,#2924,.T.);
#3665=ORIENTED_EDGE('',*,*,#2925,.T.);
#3666=ORIENTED_EDGE('',*,*,#2925,.F.);
#3667=ORIENTED_EDGE('',*,*,#2926,.T.);
#3668=ORIENTED_EDGE('',*,*,#2927,.F.);
#3669=ORIENTED_EDGE('',*,*,#2926,.F.);
#3670=ORIENTED_EDGE('',*,*,#2924,.F.);
#3671=ORIENTED_EDGE('',*,*,#2928,.T.);
#3672=ORIENTED_EDGE('',*,*,#2929,.F.);
#3673=ORIENTED_EDGE('',*,*,#2928,.F.);
#3674=ORIENTED_EDGE('',*,*,#2914,.T.);
#3675=ORIENTED_EDGE('',*,*,#2923,.T.);
#3676=ORIENTED_EDGE('',*,*,#2930,.T.);
#3677=ORIENTED_EDGE('',*,*,#2931,.T.);
#3678=ORIENTED_EDGE('',*,*,#2932,.T.);
#3679=ORIENTED_EDGE('',*,*,#2919,.T.);
#3680=ORIENTED_EDGE('',*,*,#2916,.T.);
#3681=ORIENTED_EDGE('',*,*,#2918,.T.);
#3682=ORIENTED_EDGE('',*,*,#2933,.F.);
#3683=ORIENTED_EDGE('',*,*,#2934,.T.);
#3684=ORIENTED_EDGE('',*,*,#2935,.F.);
#3685=ORIENTED_EDGE('',*,*,#2934,.F.);
#3686=ORIENTED_EDGE('',*,*,#2933,.T.);
#3687=ORIENTED_EDGE('',*,*,#2931,.F.);
#3688=ORIENTED_EDGE('',*,*,#2936,.T.);
#3689=ORIENTED_EDGE('',*,*,#2937,.F.);
#3690=ORIENTED_EDGE('',*,*,#2938,.F.);
#3691=ORIENTED_EDGE('',*,*,#2939,.F.);
#3692=ORIENTED_EDGE('',*,*,#2940,.T.);
#3693=ORIENTED_EDGE('',*,*,#2941,.F.);
#3694=ORIENTED_EDGE('',*,*,#2942,.F.);
#3695=ORIENTED_EDGE('',*,*,#2941,.T.);
#3696=ORIENTED_EDGE('',*,*,#2943,.T.);
#3697=ORIENTED_EDGE('',*,*,#2937,.T.);
#3698=ORIENTED_EDGE('',*,*,#2944,.T.);
#3699=ORIENTED_EDGE('',*,*,#2935,.T.);
#3700=ORIENTED_EDGE('',*,*,#2939,.T.);
#3701=ORIENTED_EDGE('',*,*,#2945,.T.);
#3702=ORIENTED_EDGE('',*,*,#2946,.T.);
#3703=ORIENTED_EDGE('',*,*,#2947,.T.);
#3704=ORIENTED_EDGE('',*,*,#2948,.F.);
#3705=ORIENTED_EDGE('',*,*,#2949,.T.);
#3706=ORIENTED_EDGE('',*,*,#2950,.F.);
#3707=ORIENTED_EDGE('',*,*,#2949,.F.);
#3708=ORIENTED_EDGE('',*,*,#2948,.T.);
#3709=ORIENTED_EDGE('',*,*,#2946,.F.);
#3710=ORIENTED_EDGE('',*,*,#2951,.T.);
#3711=ORIENTED_EDGE('',*,*,#2952,.F.);
#3712=ORIENTED_EDGE('',*,*,#2953,.F.);
#3713=ORIENTED_EDGE('',*,*,#2954,.F.);
#3714=ORIENTED_EDGE('',*,*,#2955,.T.);
#3715=ORIENTED_EDGE('',*,*,#2956,.F.);
#3716=ORIENTED_EDGE('',*,*,#2957,.F.);
#3717=ORIENTED_EDGE('',*,*,#2956,.T.);
#3718=ORIENTED_EDGE('',*,*,#2958,.T.);
#3719=ORIENTED_EDGE('',*,*,#2952,.T.);
#3720=ORIENTED_EDGE('',*,*,#2959,.T.);
#3721=ORIENTED_EDGE('',*,*,#2950,.T.);
#3722=ORIENTED_EDGE('',*,*,#2954,.T.);
#3723=ORIENTED_EDGE('',*,*,#2960,.T.);
#3724=ORIENTED_EDGE('',*,*,#2961,.T.);
#3725=ORIENTED_EDGE('',*,*,#2962,.T.);
#3726=ORIENTED_EDGE('',*,*,#2921,.T.);
#3727=ORIENTED_EDGE('',*,*,#2963,.T.);
#3728=ORIENTED_EDGE('',*,*,#2964,.F.);
#3729=ORIENTED_EDGE('',*,*,#2965,.F.);
#3730=ORIENTED_EDGE('',*,*,#2966,.T.);
#3731=ORIENTED_EDGE('',*,*,#2967,.T.);
#3732=ORIENTED_EDGE('',*,*,#2968,.T.);
#3733=ORIENTED_EDGE('',*,*,#2964,.T.);
#3734=ORIENTED_EDGE('',*,*,#2927,.T.);
#3735=ORIENTED_EDGE('',*,*,#2929,.T.);
#3736=ORIENTED_EDGE('',*,*,#2969,.F.);
#3737=ORIENTED_EDGE('',*,*,#2970,.T.);
#3738=ORIENTED_EDGE('',*,*,#2960,.F.);
#3739=ORIENTED_EDGE('',*,*,#2957,.T.);
#3740=ORIENTED_EDGE('',*,*,#2959,.F.);
#3741=ORIENTED_EDGE('',*,*,#2951,.F.);
#3742=ORIENTED_EDGE('',*,*,#2945,.F.);
#3743=ORIENTED_EDGE('',*,*,#2942,.T.);
#3744=ORIENTED_EDGE('',*,*,#2944,.F.);
#3745=ORIENTED_EDGE('',*,*,#2936,.F.);
#3746=ORIENTED_EDGE('',*,*,#2930,.F.);
#3747=ORIENTED_EDGE('',*,*,#2922,.T.);
#3748=ORIENTED_EDGE('',*,*,#2965,.T.);
#3749=ORIENTED_EDGE('',*,*,#2968,.F.);
#3750=ORIENTED_EDGE('',*,*,#2971,.T.);
#3751=ORIENTED_EDGE('',*,*,#2966,.F.);
#3752=ORIENTED_EDGE('',*,*,#2963,.F.);
#3753=ORIENTED_EDGE('',*,*,#2920,.T.);
#3754=ORIENTED_EDGE('',*,*,#2932,.F.);
#3755=ORIENTED_EDGE('',*,*,#2938,.T.);
#3756=ORIENTED_EDGE('',*,*,#2943,.F.);
#3757=ORIENTED_EDGE('',*,*,#2940,.F.);
#3758=ORIENTED_EDGE('',*,*,#2947,.F.);
#3759=ORIENTED_EDGE('',*,*,#2953,.T.);
#3760=ORIENTED_EDGE('',*,*,#2958,.F.);
#3761=ORIENTED_EDGE('',*,*,#2955,.F.);
#3762=ORIENTED_EDGE('',*,*,#2962,.F.);
#3763=ORIENTED_EDGE('',*,*,#2972,.F.);
#3764=ORIENTED_EDGE('',*,*,#2973,.T.);
#3765=ORIENTED_EDGE('',*,*,#2972,.T.);
#3766=ORIENTED_EDGE('',*,*,#2961,.F.);
#3767=ORIENTED_EDGE('',*,*,#2970,.F.);
#3768=ORIENTED_EDGE('',*,*,#2973,.F.);
#3769=ORIENTED_EDGE('',*,*,#2969,.T.);
#3770=ORIENTED_EDGE('',*,*,#2967,.F.);
#3771=ORIENTED_EDGE('',*,*,#2971,.F.);
#3772=ORIENTED_EDGE('',*,*,#2974,.T.);
#3773=ORIENTED_EDGE('',*,*,#2975,.T.);
#3774=ORIENTED_EDGE('',*,*,#2976,.T.);
#3775=ORIENTED_EDGE('',*,*,#2975,.F.);
#3776=ORIENTED_EDGE('',*,*,#2976,.F.);
#3777=ORIENTED_EDGE('',*,*,#2977,.T.);
#3778=ORIENTED_EDGE('',*,*,#2978,.T.);
#3779=ORIENTED_EDGE('',*,*,#2977,.F.);
#3780=ORIENTED_EDGE('',*,*,#2979,.T.);
#3781=ORIENTED_EDGE('',*,*,#2974,.F.);
#3782=ORIENTED_EDGE('',*,*,#2979,.F.);
#3783=ORIENTED_EDGE('',*,*,#2980,.T.);
#3784=ORIENTED_EDGE('',*,*,#2981,.T.);
#3785=ORIENTED_EDGE('',*,*,#2980,.F.);
#3786=ORIENTED_EDGE('',*,*,#2981,.F.);
#3787=ORIENTED_EDGE('',*,*,#2978,.F.);
#3788=ORIENTED_EDGE('',*,*,#2982,.T.);
#3789=ORIENTED_EDGE('',*,*,#2983,.T.);
#3790=ORIENTED_EDGE('',*,*,#2984,.T.);
#3791=ORIENTED_EDGE('',*,*,#2985,.F.);
#3792=ORIENTED_EDGE('',*,*,#2986,.T.);
#3793=ORIENTED_EDGE('',*,*,#2987,.T.);
#3794=ORIENTED_EDGE('',*,*,#2988,.T.);
#3795=ORIENTED_EDGE('',*,*,#2983,.F.);
#3796=ORIENTED_EDGE('',*,*,#2989,.T.);
#3797=ORIENTED_EDGE('',*,*,#2990,.T.);
#3798=ORIENTED_EDGE('',*,*,#2991,.T.);
#3799=ORIENTED_EDGE('',*,*,#2987,.F.);
#3800=ORIENTED_EDGE('',*,*,#2992,.T.);
#3801=ORIENTED_EDGE('',*,*,#2993,.T.);
#3802=ORIENTED_EDGE('',*,*,#2994,.T.);
#3803=ORIENTED_EDGE('',*,*,#2990,.F.);
#3804=ORIENTED_EDGE('',*,*,#2995,.T.);
#3805=ORIENTED_EDGE('',*,*,#2996,.T.);
#3806=ORIENTED_EDGE('',*,*,#2997,.T.);
#3807=ORIENTED_EDGE('',*,*,#2993,.F.);
#3808=ORIENTED_EDGE('',*,*,#2998,.T.);
#3809=ORIENTED_EDGE('',*,*,#2985,.T.);
#3810=ORIENTED_EDGE('',*,*,#2999,.T.);
#3811=ORIENTED_EDGE('',*,*,#2996,.F.);
#3812=ORIENTED_EDGE('',*,*,#2998,.F.);
#3813=ORIENTED_EDGE('',*,*,#2995,.F.);
#3814=ORIENTED_EDGE('',*,*,#2992,.F.);
#3815=ORIENTED_EDGE('',*,*,#2989,.F.);
#3816=ORIENTED_EDGE('',*,*,#2986,.F.);
#3817=ORIENTED_EDGE('',*,*,#2982,.F.);
#3818=ORIENTED_EDGE('',*,*,#2999,.F.);
#3819=ORIENTED_EDGE('',*,*,#2984,.F.);
#3820=ORIENTED_EDGE('',*,*,#2988,.F.);
#3821=ORIENTED_EDGE('',*,*,#2991,.F.);
#3822=ORIENTED_EDGE('',*,*,#2994,.F.);
#3823=ORIENTED_EDGE('',*,*,#2997,.F.);
#3824=ORIENTED_EDGE('',*,*,#3000,.F.);
#3825=ORIENTED_EDGE('',*,*,#3001,.F.);
#3826=ORIENTED_EDGE('',*,*,#3002,.F.);
#3827=ORIENTED_EDGE('',*,*,#3003,.T.);
#3828=ORIENTED_EDGE('',*,*,#3001,.T.);
#3829=ORIENTED_EDGE('',*,*,#3003,.F.);
#3830=ORIENTED_EDGE('',*,*,#3004,.F.);
#3831=ORIENTED_EDGE('',*,*,#3005,.T.);
#3832=ORIENTED_EDGE('',*,*,#3002,.T.);
#3833=ORIENTED_EDGE('',*,*,#3005,.F.);
#3834=ORIENTED_EDGE('',*,*,#3006,.F.);
#3835=ORIENTED_EDGE('',*,*,#3007,.T.);
#3836=ORIENTED_EDGE('',*,*,#3004,.T.);
#3837=ORIENTED_EDGE('',*,*,#3007,.F.);
#3838=ORIENTED_EDGE('',*,*,#3006,.T.);
#3839=ORIENTED_EDGE('',*,*,#3008,.F.);
#3840=ORIENTED_EDGE('',*,*,#3009,.F.);
#3841=ORIENTED_EDGE('',*,*,#3010,.T.);
#3842=ORIENTED_EDGE('',*,*,#3008,.T.);
#3843=ORIENTED_EDGE('',*,*,#3010,.F.);
#3844=ORIENTED_EDGE('',*,*,#3000,.T.);
#3845=ORIENTED_EDGE('',*,*,#3011,.T.);
#3846=ORIENTED_EDGE('',*,*,#3009,.T.);
#3847=ORIENTED_EDGE('',*,*,#3011,.F.);
#3848=ORIENTED_EDGE('',*,*,#3012,.F.);
#3849=ORIENTED_EDGE('',*,*,#3013,.T.);
#3850=ORIENTED_EDGE('',*,*,#3014,.F.);
#3851=ORIENTED_EDGE('',*,*,#3013,.F.);
#3852=ORIENTED_EDGE('',*,*,#3015,.F.);
#3853=ORIENTED_EDGE('',*,*,#3016,.T.);
#3854=ORIENTED_EDGE('',*,*,#3017,.F.);
#3855=ORIENTED_EDGE('',*,*,#3016,.F.);
#3856=ORIENTED_EDGE('',*,*,#3018,.F.);
#3857=ORIENTED_EDGE('',*,*,#3019,.T.);
#3858=ORIENTED_EDGE('',*,*,#3020,.F.);
#3859=ORIENTED_EDGE('',*,*,#3019,.F.);
#3860=ORIENTED_EDGE('',*,*,#3021,.F.);
#3861=ORIENTED_EDGE('',*,*,#3022,.T.);
#3862=ORIENTED_EDGE('',*,*,#3023,.F.);
#3863=ORIENTED_EDGE('',*,*,#3022,.F.);
#3864=ORIENTED_EDGE('',*,*,#3024,.F.);
#3865=ORIENTED_EDGE('',*,*,#3025,.T.);
#3866=ORIENTED_EDGE('',*,*,#3026,.F.);
#3867=ORIENTED_EDGE('',*,*,#3025,.F.);
#3868=ORIENTED_EDGE('',*,*,#3027,.F.);
#3869=ORIENTED_EDGE('',*,*,#3028,.T.);
#3870=ORIENTED_EDGE('',*,*,#3029,.F.);
#3871=ORIENTED_EDGE('',*,*,#3028,.F.);
#3872=ORIENTED_EDGE('',*,*,#3030,.F.);
#3873=ORIENTED_EDGE('',*,*,#3031,.T.);
#3874=ORIENTED_EDGE('',*,*,#3032,.F.);
#3875=ORIENTED_EDGE('',*,*,#3031,.F.);
#3876=ORIENTED_EDGE('',*,*,#3033,.F.);
#3877=ORIENTED_EDGE('',*,*,#3034,.T.);
#3878=ORIENTED_EDGE('',*,*,#3035,.F.);
#3879=ORIENTED_EDGE('',*,*,#3034,.F.);
#3880=ORIENTED_EDGE('',*,*,#3036,.F.);
#3881=ORIENTED_EDGE('',*,*,#3037,.T.);
#3882=ORIENTED_EDGE('',*,*,#3038,.F.);
#3883=ORIENTED_EDGE('',*,*,#3037,.F.);
#3884=ORIENTED_EDGE('',*,*,#3039,.F.);
#3885=ORIENTED_EDGE('',*,*,#3040,.T.);
#3886=ORIENTED_EDGE('',*,*,#3041,.F.);
#3887=ORIENTED_EDGE('',*,*,#3040,.F.);
#3888=ORIENTED_EDGE('',*,*,#3042,.F.);
#3889=ORIENTED_EDGE('',*,*,#3043,.T.);
#3890=ORIENTED_EDGE('',*,*,#3044,.F.);
#3891=ORIENTED_EDGE('',*,*,#3043,.F.);
#3892=ORIENTED_EDGE('',*,*,#3045,.F.);
#3893=ORIENTED_EDGE('',*,*,#3046,.T.);
#3894=ORIENTED_EDGE('',*,*,#3047,.F.);
#3895=ORIENTED_EDGE('',*,*,#3046,.F.);
#3896=ORIENTED_EDGE('',*,*,#3048,.F.);
#3897=ORIENTED_EDGE('',*,*,#3049,.T.);
#3898=ORIENTED_EDGE('',*,*,#3050,.F.);
#3899=ORIENTED_EDGE('',*,*,#3049,.F.);
#3900=ORIENTED_EDGE('',*,*,#3051,.F.);
#3901=ORIENTED_EDGE('',*,*,#3052,.T.);
#3902=ORIENTED_EDGE('',*,*,#3053,.F.);
#3903=ORIENTED_EDGE('',*,*,#3052,.F.);
#3904=ORIENTED_EDGE('',*,*,#3054,.F.);
#3905=ORIENTED_EDGE('',*,*,#3055,.T.);
#3906=ORIENTED_EDGE('',*,*,#3056,.F.);
#3907=ORIENTED_EDGE('',*,*,#3055,.F.);
#3908=ORIENTED_EDGE('',*,*,#3057,.F.);
#3909=ORIENTED_EDGE('',*,*,#3058,.T.);
#3910=ORIENTED_EDGE('',*,*,#3059,.F.);
#3911=ORIENTED_EDGE('',*,*,#3058,.F.);
#3912=ORIENTED_EDGE('',*,*,#3060,.F.);
#3913=ORIENTED_EDGE('',*,*,#3061,.T.);
#3914=ORIENTED_EDGE('',*,*,#3062,.F.);
#3915=ORIENTED_EDGE('',*,*,#3061,.F.);
#3916=ORIENTED_EDGE('',*,*,#3063,.F.);
#3917=ORIENTED_EDGE('',*,*,#3064,.T.);
#3918=ORIENTED_EDGE('',*,*,#3065,.F.);
#3919=ORIENTED_EDGE('',*,*,#3064,.F.);
#3920=ORIENTED_EDGE('',*,*,#3066,.F.);
#3921=ORIENTED_EDGE('',*,*,#3067,.T.);
#3922=ORIENTED_EDGE('',*,*,#3068,.F.);
#3923=ORIENTED_EDGE('',*,*,#3067,.F.);
#3924=ORIENTED_EDGE('',*,*,#3069,.F.);
#3925=ORIENTED_EDGE('',*,*,#3070,.T.);
#3926=ORIENTED_EDGE('',*,*,#3071,.F.);
#3927=ORIENTED_EDGE('',*,*,#3070,.F.);
#3928=ORIENTED_EDGE('',*,*,#3072,.F.);
#3929=ORIENTED_EDGE('',*,*,#3073,.T.);
#3930=ORIENTED_EDGE('',*,*,#3074,.F.);
#3931=ORIENTED_EDGE('',*,*,#3073,.F.);
#3932=ORIENTED_EDGE('',*,*,#3075,.F.);
#3933=ORIENTED_EDGE('',*,*,#3076,.T.);
#3934=ORIENTED_EDGE('',*,*,#3077,.F.);
#3935=ORIENTED_EDGE('',*,*,#3076,.F.);
#3936=ORIENTED_EDGE('',*,*,#3078,.F.);
#3937=ORIENTED_EDGE('',*,*,#3079,.T.);
#3938=ORIENTED_EDGE('',*,*,#3080,.F.);
#3939=ORIENTED_EDGE('',*,*,#3079,.F.);
#3940=ORIENTED_EDGE('',*,*,#3081,.F.);
#3941=ORIENTED_EDGE('',*,*,#3082,.T.);
#3942=ORIENTED_EDGE('',*,*,#3083,.F.);
#3943=ORIENTED_EDGE('',*,*,#3082,.F.);
#3944=ORIENTED_EDGE('',*,*,#3084,.F.);
#3945=ORIENTED_EDGE('',*,*,#3085,.T.);
#3946=ORIENTED_EDGE('',*,*,#3086,.F.);
#3947=ORIENTED_EDGE('',*,*,#3085,.F.);
#3948=ORIENTED_EDGE('',*,*,#3087,.F.);
#3949=ORIENTED_EDGE('',*,*,#3088,.T.);
#3950=ORIENTED_EDGE('',*,*,#3089,.F.);
#3951=ORIENTED_EDGE('',*,*,#3088,.F.);
#3952=ORIENTED_EDGE('',*,*,#3090,.F.);
#3953=ORIENTED_EDGE('',*,*,#3091,.T.);
#3954=ORIENTED_EDGE('',*,*,#3092,.F.);
#3955=ORIENTED_EDGE('',*,*,#3091,.F.);
#3956=ORIENTED_EDGE('',*,*,#3093,.F.);
#3957=ORIENTED_EDGE('',*,*,#3094,.T.);
#3958=ORIENTED_EDGE('',*,*,#3095,.F.);
#3959=ORIENTED_EDGE('',*,*,#3094,.F.);
#3960=ORIENTED_EDGE('',*,*,#3096,.T.);
#3961=ORIENTED_EDGE('',*,*,#3097,.T.);
#3962=ORIENTED_EDGE('',*,*,#3098,.F.);
#3963=ORIENTED_EDGE('',*,*,#3099,.F.);
#3964=ORIENTED_EDGE('',*,*,#3100,.T.);
#3965=ORIENTED_EDGE('',*,*,#3099,.T.);
#3966=ORIENTED_EDGE('',*,*,#3101,.F.);
#3967=ORIENTED_EDGE('',*,*,#3102,.F.);
#3968=ORIENTED_EDGE('',*,*,#3020,.T.);
#3969=ORIENTED_EDGE('',*,*,#3023,.T.);
#3970=ORIENTED_EDGE('',*,*,#3026,.T.);
#3971=ORIENTED_EDGE('',*,*,#3029,.T.);
#3972=ORIENTED_EDGE('',*,*,#3038,.T.);
#3973=ORIENTED_EDGE('',*,*,#3041,.T.);
#3974=ORIENTED_EDGE('',*,*,#3044,.T.);
#3975=ORIENTED_EDGE('',*,*,#3047,.T.);
#3976=ORIENTED_EDGE('',*,*,#3050,.T.);
#3977=ORIENTED_EDGE('',*,*,#3053,.T.);
#3978=ORIENTED_EDGE('',*,*,#3056,.T.);
#3979=ORIENTED_EDGE('',*,*,#3059,.T.);
#3980=ORIENTED_EDGE('',*,*,#3062,.T.);
#3981=ORIENTED_EDGE('',*,*,#3065,.T.);
#3982=ORIENTED_EDGE('',*,*,#3068,.T.);
#3983=ORIENTED_EDGE('',*,*,#3071,.T.);
#3984=ORIENTED_EDGE('',*,*,#3074,.T.);
#3985=ORIENTED_EDGE('',*,*,#3077,.T.);
#3986=ORIENTED_EDGE('',*,*,#3080,.T.);
#3987=ORIENTED_EDGE('',*,*,#3083,.T.);
#3988=ORIENTED_EDGE('',*,*,#3086,.T.);
#3989=ORIENTED_EDGE('',*,*,#3089,.T.);
#3990=ORIENTED_EDGE('',*,*,#3092,.T.);
#3991=ORIENTED_EDGE('',*,*,#3095,.T.);
#3992=ORIENTED_EDGE('',*,*,#3035,.T.);
#3993=ORIENTED_EDGE('',*,*,#3032,.T.);
#3994=ORIENTED_EDGE('',*,*,#3017,.T.);
#3995=ORIENTED_EDGE('',*,*,#3014,.T.);
#3996=ORIENTED_EDGE('',*,*,#3103,.T.);
#3997=ORIENTED_EDGE('',*,*,#3102,.T.);
#3998=ORIENTED_EDGE('',*,*,#3104,.F.);
#3999=ORIENTED_EDGE('',*,*,#3105,.F.);
#4000=ORIENTED_EDGE('',*,*,#3106,.T.);
#4001=ORIENTED_EDGE('',*,*,#3105,.T.);
#4002=ORIENTED_EDGE('',*,*,#3107,.F.);
#4003=ORIENTED_EDGE('',*,*,#3097,.F.);
#4004=ORIENTED_EDGE('',*,*,#3018,.T.);
#4005=ORIENTED_EDGE('',*,*,#3021,.T.);
#4006=ORIENTED_EDGE('',*,*,#3024,.T.);
#4007=ORIENTED_EDGE('',*,*,#3027,.T.);
#4008=ORIENTED_EDGE('',*,*,#3036,.T.);
#4009=ORIENTED_EDGE('',*,*,#3039,.T.);
#4010=ORIENTED_EDGE('',*,*,#3042,.T.);
#4011=ORIENTED_EDGE('',*,*,#3045,.T.);
#4012=ORIENTED_EDGE('',*,*,#3048,.T.);
#4013=ORIENTED_EDGE('',*,*,#3051,.T.);
#4014=ORIENTED_EDGE('',*,*,#3054,.T.);
#4015=ORIENTED_EDGE('',*,*,#3057,.T.);
#4016=ORIENTED_EDGE('',*,*,#3060,.T.);
#4017=ORIENTED_EDGE('',*,*,#3063,.T.);
#4018=ORIENTED_EDGE('',*,*,#3066,.T.);
#4019=ORIENTED_EDGE('',*,*,#3069,.T.);
#4020=ORIENTED_EDGE('',*,*,#3072,.T.);
#4021=ORIENTED_EDGE('',*,*,#3075,.T.);
#4022=ORIENTED_EDGE('',*,*,#3078,.T.);
#4023=ORIENTED_EDGE('',*,*,#3081,.T.);
#4024=ORIENTED_EDGE('',*,*,#3084,.T.);
#4025=ORIENTED_EDGE('',*,*,#3087,.T.);
#4026=ORIENTED_EDGE('',*,*,#3090,.T.);
#4027=ORIENTED_EDGE('',*,*,#3093,.T.);
#4028=ORIENTED_EDGE('',*,*,#3033,.T.);
#4029=ORIENTED_EDGE('',*,*,#3030,.T.);
#4030=ORIENTED_EDGE('',*,*,#3015,.T.);
#4031=ORIENTED_EDGE('',*,*,#3012,.T.);
#4032=ORIENTED_EDGE('',*,*,#3107,.T.);
#4033=ORIENTED_EDGE('',*,*,#3104,.T.);
#4034=ORIENTED_EDGE('',*,*,#3101,.T.);
#4035=ORIENTED_EDGE('',*,*,#3098,.T.);
#4036=ORIENTED_EDGE('',*,*,#3106,.F.);
#4037=ORIENTED_EDGE('',*,*,#3096,.F.);
#4038=ORIENTED_EDGE('',*,*,#3100,.F.);
#4039=ORIENTED_EDGE('',*,*,#3103,.F.);
#4040=ORIENTED_EDGE('',*,*,#3108,.F.);
#4041=ORIENTED_EDGE('',*,*,#3109,.T.);
#4042=ORIENTED_EDGE('',*,*,#3110,.F.);
#4043=ORIENTED_EDGE('',*,*,#3109,.F.);
#4044=ORIENTED_EDGE('',*,*,#3111,.F.);
#4045=ORIENTED_EDGE('',*,*,#3112,.T.);
#4046=ORIENTED_EDGE('',*,*,#3113,.F.);
#4047=ORIENTED_EDGE('',*,*,#3112,.F.);
#4048=ORIENTED_EDGE('',*,*,#3114,.T.);
#4049=ORIENTED_EDGE('',*,*,#3115,.T.);
#4050=ORIENTED_EDGE('',*,*,#3116,.F.);
#4051=ORIENTED_EDGE('',*,*,#3117,.F.);
#4052=ORIENTED_EDGE('',*,*,#3118,.T.);
#4053=ORIENTED_EDGE('',*,*,#3117,.T.);
#4054=ORIENTED_EDGE('',*,*,#3119,.F.);
#4055=ORIENTED_EDGE('',*,*,#3120,.F.);
#4056=ORIENTED_EDGE('',*,*,#3110,.T.);
#4057=ORIENTED_EDGE('',*,*,#3113,.T.);
#4058=ORIENTED_EDGE('',*,*,#3121,.T.);
#4059=ORIENTED_EDGE('',*,*,#3120,.T.);
#4060=ORIENTED_EDGE('',*,*,#3122,.F.);
#4061=ORIENTED_EDGE('',*,*,#3123,.F.);
#4062=ORIENTED_EDGE('',*,*,#3124,.T.);
#4063=ORIENTED_EDGE('',*,*,#3123,.T.);
#4064=ORIENTED_EDGE('',*,*,#3125,.F.);
#4065=ORIENTED_EDGE('',*,*,#3115,.F.);
#4066=ORIENTED_EDGE('',*,*,#3108,.T.);
#4067=ORIENTED_EDGE('',*,*,#3111,.T.);
#4068=ORIENTED_EDGE('',*,*,#3125,.T.);
#4069=ORIENTED_EDGE('',*,*,#3122,.T.);
#4070=ORIENTED_EDGE('',*,*,#3119,.T.);
#4071=ORIENTED_EDGE('',*,*,#3116,.T.);
#4072=ORIENTED_EDGE('',*,*,#3124,.F.);
#4073=ORIENTED_EDGE('',*,*,#3114,.F.);
#4074=ORIENTED_EDGE('',*,*,#3118,.F.);
#4075=ORIENTED_EDGE('',*,*,#3121,.F.);
#4076=ORIENTED_EDGE('',*,*,#3126,.F.);
#4077=ORIENTED_EDGE('',*,*,#3127,.T.);
#4078=ORIENTED_EDGE('',*,*,#3128,.F.);
#4079=ORIENTED_EDGE('',*,*,#3127,.F.);
#4080=ORIENTED_EDGE('',*,*,#3129,.F.);
#4081=ORIENTED_EDGE('',*,*,#3130,.T.);
#4082=ORIENTED_EDGE('',*,*,#3126,.T.);
#4083=ORIENTED_EDGE('',*,*,#3130,.F.);
#4084=ORIENTED_EDGE('',*,*,#3129,.T.);
#4085=ORIENTED_EDGE('',*,*,#3131,.F.);
#4086=ORIENTED_EDGE('',*,*,#3132,.T.);
#4087=ORIENTED_EDGE('',*,*,#3133,.F.);
#4088=ORIENTED_EDGE('',*,*,#3134,.F.);
#4089=ORIENTED_EDGE('',*,*,#3135,.F.);
#4090=ORIENTED_EDGE('',*,*,#3136,.F.);
#4091=ORIENTED_EDGE('',*,*,#3137,.F.);
#4092=ORIENTED_EDGE('',*,*,#3138,.F.);
#4093=ORIENTED_EDGE('',*,*,#3132,.F.);
#4094=ORIENTED_EDGE('',*,*,#3137,.T.);
#4095=ORIENTED_EDGE('',*,*,#3139,.F.);
#4096=ORIENTED_EDGE('',*,*,#3140,.T.);
#4097=ORIENTED_EDGE('',*,*,#3141,.T.);
#4098=ORIENTED_EDGE('',*,*,#3136,.T.);
#4099=ORIENTED_EDGE('',*,*,#3142,.F.);
#4100=ORIENTED_EDGE('',*,*,#3143,.T.);
#4101=ORIENTED_EDGE('',*,*,#3139,.T.);
#4102=ORIENTED_EDGE('',*,*,#3135,.T.);
#4103=ORIENTED_EDGE('',*,*,#3144,.F.);
#4104=ORIENTED_EDGE('',*,*,#3145,.T.);
#4105=ORIENTED_EDGE('',*,*,#3142,.T.);
#4106=ORIENTED_EDGE('',*,*,#3134,.T.);
#4107=ORIENTED_EDGE('',*,*,#3146,.F.);
#4108=ORIENTED_EDGE('',*,*,#3147,.T.);
#4109=ORIENTED_EDGE('',*,*,#3144,.T.);
#4110=ORIENTED_EDGE('',*,*,#3133,.T.);
#4111=ORIENTED_EDGE('',*,*,#3148,.F.);
#4112=ORIENTED_EDGE('',*,*,#3149,.T.);
#4113=ORIENTED_EDGE('',*,*,#3146,.T.);
#4114=ORIENTED_EDGE('',*,*,#3138,.T.);
#4115=ORIENTED_EDGE('',*,*,#3141,.F.);
#4116=ORIENTED_EDGE('',*,*,#3150,.T.);
#4117=ORIENTED_EDGE('',*,*,#3148,.T.);
#4118=ORIENTED_EDGE('',*,*,#3131,.T.);
#4119=ORIENTED_EDGE('',*,*,#3145,.F.);
#4120=ORIENTED_EDGE('',*,*,#3147,.F.);
#4121=ORIENTED_EDGE('',*,*,#3149,.F.);
#4122=ORIENTED_EDGE('',*,*,#3150,.F.);
#4123=ORIENTED_EDGE('',*,*,#3140,.F.);
#4124=ORIENTED_EDGE('',*,*,#3143,.F.);
#4125=ORIENTED_EDGE('',*,*,#3128,.T.);
#4126=ORIENTED_EDGE('',*,*,#3151,.F.);
#4127=ORIENTED_EDGE('',*,*,#3152,.F.);
#4128=ORIENTED_EDGE('',*,*,#3153,.T.);
#4129=ORIENTED_EDGE('',*,*,#3154,.F.);
#4130=ORIENTED_EDGE('',*,*,#3153,.F.);
#4131=ORIENTED_EDGE('',*,*,#3155,.F.);
#4132=ORIENTED_EDGE('',*,*,#3156,.F.);
#4133=ORIENTED_EDGE('',*,*,#3157,.F.);
#4134=ORIENTED_EDGE('',*,*,#3158,.F.);
#4135=ORIENTED_EDGE('',*,*,#3159,.F.);
#4136=ORIENTED_EDGE('',*,*,#3160,.T.);
#4137=ORIENTED_EDGE('',*,*,#3161,.F.);
#4138=ORIENTED_EDGE('',*,*,#3162,.F.);
#4139=ORIENTED_EDGE('',*,*,#3163,.F.);
#4140=ORIENTED_EDGE('',*,*,#3164,.F.);
#4141=ORIENTED_EDGE('',*,*,#3165,.F.);
#4142=ORIENTED_EDGE('',*,*,#3166,.F.);
#4143=ORIENTED_EDGE('',*,*,#3160,.F.);
#4144=ORIENTED_EDGE('',*,*,#3156,.T.);
#4145=ORIENTED_EDGE('',*,*,#3167,.T.);
#4146=ORIENTED_EDGE('',*,*,#3165,.T.);
#4147=ORIENTED_EDGE('',*,*,#3168,.F.);
#4148=ORIENTED_EDGE('',*,*,#3155,.T.);
#4149=ORIENTED_EDGE('',*,*,#3169,.T.);
#4150=ORIENTED_EDGE('',*,*,#3166,.T.);
#4151=ORIENTED_EDGE('',*,*,#3167,.F.);
#4152=ORIENTED_EDGE('',*,*,#3152,.T.);
#4153=ORIENTED_EDGE('',*,*,#3170,.T.);
#4154=ORIENTED_EDGE('',*,*,#3161,.T.);
#4155=ORIENTED_EDGE('',*,*,#3169,.F.);
#4156=ORIENTED_EDGE('',*,*,#3171,.F.);
#4157=ORIENTED_EDGE('',*,*,#3172,.T.);
#4158=ORIENTED_EDGE('',*,*,#3173,.T.);
#4159=ORIENTED_EDGE('',*,*,#3172,.F.);
#4160=ORIENTED_EDGE('',*,*,#3151,.T.);
#4161=ORIENTED_EDGE('',*,*,#3174,.T.);
#4162=ORIENTED_EDGE('',*,*,#3162,.T.);
#4163=ORIENTED_EDGE('',*,*,#3170,.F.);
#4164=ORIENTED_EDGE('',*,*,#3157,.T.);
#4165=ORIENTED_EDGE('',*,*,#3168,.T.);
#4166=ORIENTED_EDGE('',*,*,#3164,.T.);
#4167=ORIENTED_EDGE('',*,*,#3175,.F.);
#4168=ORIENTED_EDGE('',*,*,#3158,.T.);
#4169=ORIENTED_EDGE('',*,*,#3175,.T.);
#4170=ORIENTED_EDGE('',*,*,#3163,.T.);
#4171=ORIENTED_EDGE('',*,*,#3174,.F.);
#4172=ORIENTED_EDGE('',*,*,#3159,.T.);
#4173=ORIENTED_EDGE('',*,*,#3171,.T.);
#4174=ORIENTED_EDGE('',*,*,#3154,.T.);
#4175=ORIENTED_EDGE('',*,*,#3173,.F.);
#4176=ORIENTED_EDGE('',*,*,#3176,.F.);
#4177=ORIENTED_EDGE('',*,*,#3177,.T.);
#4178=ORIENTED_EDGE('',*,*,#3178,.F.);
#4179=ORIENTED_EDGE('',*,*,#3177,.F.);
#4180=ORIENTED_EDGE('',*,*,#3176,.T.);
#4181=ORIENTED_EDGE('',*,*,#3179,.F.);
#4182=ORIENTED_EDGE('',*,*,#3180,.T.);
#4183=ORIENTED_EDGE('',*,*,#3181,.T.);
#4184=ORIENTED_EDGE('',*,*,#3180,.F.);
#4185=ORIENTED_EDGE('',*,*,#3179,.T.);
#4186=ORIENTED_EDGE('',*,*,#3178,.T.);
#4187=ORIENTED_EDGE('',*,*,#3181,.F.);
#4188=ORIENTED_EDGE('',*,*,#3182,.F.);
#4189=ORIENTED_EDGE('',*,*,#3183,.F.);
#4190=ORIENTED_EDGE('',*,*,#3184,.T.);
#4191=ORIENTED_EDGE('',*,*,#3182,.T.);
#4192=ORIENTED_EDGE('',*,*,#3184,.F.);
#4193=ORIENTED_EDGE('',*,*,#3185,.F.);
#4194=ORIENTED_EDGE('',*,*,#3186,.T.);
#4195=ORIENTED_EDGE('',*,*,#3183,.T.);
#4196=ORIENTED_EDGE('',*,*,#3186,.F.);
#4197=ORIENTED_EDGE('',*,*,#3185,.T.);
#4198=ORIENTED_EDGE('',*,*,#3187,.F.);
#4199=ORIENTED_EDGE('',*,*,#3188,.F.);
#4200=ORIENTED_EDGE('',*,*,#3189,.F.);
#4201=ORIENTED_EDGE('',*,*,#3190,.F.);
#4202=ORIENTED_EDGE('',*,*,#3191,.F.);
#4203=ORIENTED_EDGE('',*,*,#3192,.F.);
#4204=ORIENTED_EDGE('',*,*,#3193,.F.);
#4205=ORIENTED_EDGE('',*,*,#3188,.T.);
#4206=ORIENTED_EDGE('',*,*,#3189,.T.);
#4207=ORIENTED_EDGE('',*,*,#3187,.T.);
#4208=ORIENTED_EDGE('',*,*,#3193,.T.);
#4209=ORIENTED_EDGE('',*,*,#3194,.F.);
#4210=ORIENTED_EDGE('',*,*,#3195,.T.);
#4211=ORIENTED_EDGE('',*,*,#3196,.T.);
#4212=ORIENTED_EDGE('',*,*,#3197,.T.);
#4213=ORIENTED_EDGE('',*,*,#3198,.T.);
#4214=ORIENTED_EDGE('',*,*,#3197,.F.);
#4215=ORIENTED_EDGE('',*,*,#3199,.T.);
#4216=ORIENTED_EDGE('',*,*,#3200,.T.);
#4217=ORIENTED_EDGE('',*,*,#3201,.F.);
#4218=ORIENTED_EDGE('',*,*,#3192,.T.);
#4219=ORIENTED_EDGE('',*,*,#3202,.F.);
#4220=ORIENTED_EDGE('',*,*,#3203,.T.);
#4221=ORIENTED_EDGE('',*,*,#3194,.T.);
#4222=ORIENTED_EDGE('',*,*,#3200,.F.);
#4223=ORIENTED_EDGE('',*,*,#3204,.F.);
#4224=ORIENTED_EDGE('',*,*,#3195,.F.);
#4225=ORIENTED_EDGE('',*,*,#3203,.F.);
#4226=ORIENTED_EDGE('',*,*,#3205,.F.);
#4227=ORIENTED_EDGE('',*,*,#3206,.F.);
#4228=ORIENTED_EDGE('',*,*,#3196,.F.);
#4229=ORIENTED_EDGE('',*,*,#3204,.T.);
#4230=ORIENTED_EDGE('',*,*,#3199,.F.);
#4231=ORIENTED_EDGE('',*,*,#3191,.T.);
#4232=ORIENTED_EDGE('',*,*,#3207,.T.);
#4233=ORIENTED_EDGE('',*,*,#3205,.T.);
#4234=ORIENTED_EDGE('',*,*,#3202,.T.);
#4235=ORIENTED_EDGE('',*,*,#3198,.F.);
#4236=ORIENTED_EDGE('',*,*,#3190,.T.);
#4237=ORIENTED_EDGE('',*,*,#3201,.T.);
#4238=ORIENTED_EDGE('',*,*,#3206,.T.);
#4239=ORIENTED_EDGE('',*,*,#3207,.F.);
#4240=ORIENTED_EDGE('',*,*,#3208,.T.);
#4241=ORIENTED_EDGE('',*,*,#3209,.T.);
#4242=ORIENTED_EDGE('',*,*,#3210,.T.);
#4243=ORIENTED_EDGE('',*,*,#3211,.F.);
#4244=ORIENTED_EDGE('',*,*,#3212,.T.);
#4245=ORIENTED_EDGE('',*,*,#3213,.T.);
#4246=ORIENTED_EDGE('',*,*,#3214,.T.);
#4247=ORIENTED_EDGE('',*,*,#3209,.F.);
#4248=ORIENTED_EDGE('',*,*,#3215,.T.);
#4249=ORIENTED_EDGE('',*,*,#3216,.T.);
#4250=ORIENTED_EDGE('',*,*,#3217,.T.);
#4251=ORIENTED_EDGE('',*,*,#3213,.F.);
#4252=ORIENTED_EDGE('',*,*,#3218,.T.);
#4253=ORIENTED_EDGE('',*,*,#3219,.T.);
#4254=ORIENTED_EDGE('',*,*,#3220,.T.);
#4255=ORIENTED_EDGE('',*,*,#3216,.F.);
#4256=ORIENTED_EDGE('',*,*,#3221,.T.);
#4257=ORIENTED_EDGE('',*,*,#3222,.T.);
#4258=ORIENTED_EDGE('',*,*,#3223,.T.);
#4259=ORIENTED_EDGE('',*,*,#3219,.F.);
#4260=ORIENTED_EDGE('',*,*,#3224,.T.);
#4261=ORIENTED_EDGE('',*,*,#3211,.T.);
#4262=ORIENTED_EDGE('',*,*,#3225,.T.);
#4263=ORIENTED_EDGE('',*,*,#3222,.F.);
#4264=ORIENTED_EDGE('',*,*,#3224,.F.);
#4265=ORIENTED_EDGE('',*,*,#3221,.F.);
#4266=ORIENTED_EDGE('',*,*,#3218,.F.);
#4267=ORIENTED_EDGE('',*,*,#3215,.F.);
#4268=ORIENTED_EDGE('',*,*,#3212,.F.);
#4269=ORIENTED_EDGE('',*,*,#3208,.F.);
#4270=ORIENTED_EDGE('',*,*,#3225,.F.);
#4271=ORIENTED_EDGE('',*,*,#3210,.F.);
#4272=ORIENTED_EDGE('',*,*,#3214,.F.);
#4273=ORIENTED_EDGE('',*,*,#3217,.F.);
#4274=ORIENTED_EDGE('',*,*,#3220,.F.);
#4275=ORIENTED_EDGE('',*,*,#3223,.F.);
#4276=ORIENTED_EDGE('',*,*,#3226,.F.);
#4277=ORIENTED_EDGE('',*,*,#3227,.F.);
#4278=ORIENTED_EDGE('',*,*,#3228,.F.);
#4279=ORIENTED_EDGE('',*,*,#3229,.T.);
#4280=ORIENTED_EDGE('',*,*,#3227,.T.);
#4281=ORIENTED_EDGE('',*,*,#3229,.F.);
#4282=ORIENTED_EDGE('',*,*,#3230,.F.);
#4283=ORIENTED_EDGE('',*,*,#3231,.T.);
#4284=ORIENTED_EDGE('',*,*,#3228,.T.);
#4285=ORIENTED_EDGE('',*,*,#3231,.F.);
#4286=ORIENTED_EDGE('',*,*,#3232,.F.);
#4287=ORIENTED_EDGE('',*,*,#3233,.T.);
#4288=ORIENTED_EDGE('',*,*,#3230,.T.);
#4289=ORIENTED_EDGE('',*,*,#3233,.F.);
#4290=ORIENTED_EDGE('',*,*,#3232,.T.);
#4291=ORIENTED_EDGE('',*,*,#3234,.F.);
#4292=ORIENTED_EDGE('',*,*,#3235,.F.);
#4293=ORIENTED_EDGE('',*,*,#3236,.T.);
#4294=ORIENTED_EDGE('',*,*,#3234,.T.);
#4295=ORIENTED_EDGE('',*,*,#3236,.F.);
#4296=ORIENTED_EDGE('',*,*,#3226,.T.);
#4297=ORIENTED_EDGE('',*,*,#3237,.T.);
#4298=ORIENTED_EDGE('',*,*,#3235,.T.);
#4299=ORIENTED_EDGE('',*,*,#3237,.F.);
#4300=ORIENTED_EDGE('',*,*,#3238,.F.);
#4301=ORIENTED_EDGE('',*,*,#3239,.T.);
#4302=ORIENTED_EDGE('',*,*,#3240,.F.);
#4303=ORIENTED_EDGE('',*,*,#3239,.F.);
#4304=ORIENTED_EDGE('',*,*,#3241,.F.);
#4305=ORIENTED_EDGE('',*,*,#3242,.T.);
#4306=ORIENTED_EDGE('',*,*,#3243,.F.);
#4307=ORIENTED_EDGE('',*,*,#3242,.F.);
#4308=ORIENTED_EDGE('',*,*,#3244,.F.);
#4309=ORIENTED_EDGE('',*,*,#3245,.F.);
#4310=ORIENTED_EDGE('',*,*,#3246,.F.);
#4311=ORIENTED_EDGE('',*,*,#3247,.T.);
#4312=ORIENTED_EDGE('',*,*,#3247,.F.);
#4313=ORIENTED_EDGE('',*,*,#3248,.F.);
#4314=ORIENTED_EDGE('',*,*,#3249,.F.);
#4315=ORIENTED_EDGE('',*,*,#3250,.F.);
#4316=ORIENTED_EDGE('',*,*,#3238,.T.);
#4317=ORIENTED_EDGE('',*,*,#3246,.T.);
#4318=ORIENTED_EDGE('',*,*,#3251,.F.);
#4319=ORIENTED_EDGE('',*,*,#3252,.F.);
#4320=ORIENTED_EDGE('',*,*,#3248,.T.);
#4321=ORIENTED_EDGE('',*,*,#3253,.T.);
#4322=ORIENTED_EDGE('',*,*,#3254,.F.);
#4323=ORIENTED_EDGE('',*,*,#3251,.T.);
#4324=ORIENTED_EDGE('',*,*,#3245,.T.);
#4325=ORIENTED_EDGE('',*,*,#3240,.T.);
#4326=ORIENTED_EDGE('',*,*,#3244,.T.);
#4327=ORIENTED_EDGE('',*,*,#3250,.T.);
#4328=ORIENTED_EDGE('',*,*,#3255,.F.);
#4329=ORIENTED_EDGE('',*,*,#3253,.F.);
#4330=ORIENTED_EDGE('',*,*,#3256,.F.);
#4331=ORIENTED_EDGE('',*,*,#3257,.T.);
#4332=ORIENTED_EDGE('',*,*,#3258,.F.);
#4333=ORIENTED_EDGE('',*,*,#3257,.F.);
#4334=ORIENTED_EDGE('',*,*,#3259,.F.);
#4335=ORIENTED_EDGE('',*,*,#3260,.T.);
#4336=ORIENTED_EDGE('',*,*,#3261,.F.);
#4337=ORIENTED_EDGE('',*,*,#3260,.F.);
#4338=ORIENTED_EDGE('',*,*,#3262,.F.);
#4339=ORIENTED_EDGE('',*,*,#3263,.T.);
#4340=ORIENTED_EDGE('',*,*,#3264,.F.);
#4341=ORIENTED_EDGE('',*,*,#3265,.F.);
#4342=ORIENTED_EDGE('',*,*,#3266,.T.);
#4343=ORIENTED_EDGE('',*,*,#3267,.T.);
#4344=ORIENTED_EDGE('',*,*,#3268,.T.);
#4345=ORIENTED_EDGE('',*,*,#3269,.T.);
#4346=ORIENTED_EDGE('',*,*,#3261,.T.);
#4347=ORIENTED_EDGE('',*,*,#3270,.F.);
#4348=ORIENTED_EDGE('',*,*,#3271,.T.);
#4349=ORIENTED_EDGE('',*,*,#3267,.F.);
#4350=ORIENTED_EDGE('',*,*,#3272,.F.);
#4351=ORIENTED_EDGE('',*,*,#3264,.T.);
#4352=ORIENTED_EDGE('',*,*,#3273,.T.);
#4353=ORIENTED_EDGE('',*,*,#3270,.T.);
#4354=ORIENTED_EDGE('',*,*,#3274,.T.);
#4355=ORIENTED_EDGE('',*,*,#3259,.T.);
#4356=ORIENTED_EDGE('',*,*,#3275,.T.);
#4357=ORIENTED_EDGE('',*,*,#3276,.F.);
#4358=ORIENTED_EDGE('',*,*,#3277,.F.);
#4359=ORIENTED_EDGE('',*,*,#3278,.F.);
#4360=ORIENTED_EDGE('',*,*,#3279,.T.);
#4361=ORIENTED_EDGE('',*,*,#3280,.F.);
#4362=ORIENTED_EDGE('',*,*,#3281,.F.);
#4363=ORIENTED_EDGE('',*,*,#3276,.T.);
#4364=ORIENTED_EDGE('',*,*,#3282,.T.);
#4365=ORIENTED_EDGE('',*,*,#3283,.T.);
#4366=ORIENTED_EDGE('',*,*,#3284,.F.);
#4367=ORIENTED_EDGE('',*,*,#3280,.T.);
#4368=ORIENTED_EDGE('',*,*,#3285,.T.);
#4369=ORIENTED_EDGE('',*,*,#3278,.T.);
#4370=ORIENTED_EDGE('',*,*,#3286,.F.);
#4371=ORIENTED_EDGE('',*,*,#3283,.F.);
#4372=ORIENTED_EDGE('',*,*,#3287,.F.);
#4373=ORIENTED_EDGE('',*,*,#3288,.T.);
#4374=ORIENTED_EDGE('',*,*,#3289,.T.);
#4375=ORIENTED_EDGE('',*,*,#3288,.F.);
#4376=ORIENTED_EDGE('',*,*,#3252,.T.);
#4377=ORIENTED_EDGE('',*,*,#3254,.T.);
#4378=ORIENTED_EDGE('',*,*,#3255,.T.);
#4379=ORIENTED_EDGE('',*,*,#3249,.T.);
#4380=ORIENTED_EDGE('',*,*,#3281,.T.);
#4381=ORIENTED_EDGE('',*,*,#3284,.T.);
#4382=ORIENTED_EDGE('',*,*,#3286,.T.);
#4383=ORIENTED_EDGE('',*,*,#3277,.T.);
#4384=ORIENTED_EDGE('',*,*,#3287,.T.);
#4385=ORIENTED_EDGE('',*,*,#3243,.T.);
#4386=ORIENTED_EDGE('',*,*,#3289,.F.);
#4387=ORIENTED_EDGE('',*,*,#3241,.T.);
#4388=ORIENTED_EDGE('',*,*,#3290,.F.);
#4389=ORIENTED_EDGE('',*,*,#3291,.F.);
#4390=ORIENTED_EDGE('',*,*,#3292,.F.);
#4391=ORIENTED_EDGE('',*,*,#3293,.T.);
#4392=ORIENTED_EDGE('',*,*,#3268,.F.);
#4393=ORIENTED_EDGE('',*,*,#3271,.F.);
#4394=ORIENTED_EDGE('',*,*,#3273,.F.);
#4395=ORIENTED_EDGE('',*,*,#3263,.F.);
#4396=ORIENTED_EDGE('',*,*,#3262,.T.);
#4397=ORIENTED_EDGE('',*,*,#3294,.T.);
#4398=ORIENTED_EDGE('',*,*,#3295,.T.);
#4399=ORIENTED_EDGE('',*,*,#3290,.T.);
#4400=ORIENTED_EDGE('',*,*,#3258,.T.);
#4401=ORIENTED_EDGE('',*,*,#3296,.F.);
#4402=ORIENTED_EDGE('',*,*,#3297,.T.);
#4403=ORIENTED_EDGE('',*,*,#3269,.F.);
#4404=ORIENTED_EDGE('',*,*,#3293,.F.);
#4405=ORIENTED_EDGE('',*,*,#3282,.F.);
#4406=ORIENTED_EDGE('',*,*,#3279,.F.);
#4407=ORIENTED_EDGE('',*,*,#3275,.F.);
#4408=ORIENTED_EDGE('',*,*,#3285,.F.);
#4409=ORIENTED_EDGE('',*,*,#3298,.F.);
#4410=ORIENTED_EDGE('',*,*,#3291,.T.);
#4411=ORIENTED_EDGE('',*,*,#3295,.F.);
#4412=ORIENTED_EDGE('',*,*,#3299,.F.);
#4413=ORIENTED_EDGE('',*,*,#3300,.F.);
#4414=ORIENTED_EDGE('',*,*,#3299,.T.);
#4415=ORIENTED_EDGE('',*,*,#3294,.F.);
#4416=ORIENTED_EDGE('',*,*,#3265,.T.);
#4417=ORIENTED_EDGE('',*,*,#3274,.F.);
#4418=ORIENTED_EDGE('',*,*,#3272,.T.);
#4419=ORIENTED_EDGE('',*,*,#3266,.F.);
#4420=ORIENTED_EDGE('',*,*,#3297,.F.);
#4421=ORIENTED_EDGE('',*,*,#3292,.T.);
#4422=ORIENTED_EDGE('',*,*,#3298,.T.);
#4423=ORIENTED_EDGE('',*,*,#3300,.T.);
#4424=ORIENTED_EDGE('',*,*,#3296,.T.);
#4425=ORIENTED_EDGE('',*,*,#3256,.T.);
#4426=ORIENTED_EDGE('',*,*,#3301,.F.);
#4427=ORIENTED_EDGE('',*,*,#3302,.T.);
#4428=ORIENTED_EDGE('',*,*,#3303,.F.);
#4429=ORIENTED_EDGE('',*,*,#3302,.F.);
#4430=ORIENTED_EDGE('',*,*,#3301,.T.);
#4431=ORIENTED_EDGE('',*,*,#3304,.F.);
#4432=ORIENTED_EDGE('',*,*,#3305,.T.);
#4433=ORIENTED_EDGE('',*,*,#3306,.T.);
#4434=ORIENTED_EDGE('',*,*,#3305,.F.);
#4435=ORIENTED_EDGE('',*,*,#3304,.T.);
#4436=ORIENTED_EDGE('',*,*,#3303,.T.);
#4437=ORIENTED_EDGE('',*,*,#3306,.F.);
#4438=ORIENTED_EDGE('',*,*,#3307,.T.);
#4439=ORIENTED_EDGE('',*,*,#3308,.T.);
#4440=ORIENTED_EDGE('',*,*,#3309,.T.);
#4441=ORIENTED_EDGE('',*,*,#3310,.F.);
#4442=ORIENTED_EDGE('',*,*,#3311,.T.);
#4443=ORIENTED_EDGE('',*,*,#3312,.T.);
#4444=ORIENTED_EDGE('',*,*,#3313,.T.);
#4445=ORIENTED_EDGE('',*,*,#3308,.F.);
#4446=ORIENTED_EDGE('',*,*,#3314,.T.);
#4447=ORIENTED_EDGE('',*,*,#3315,.T.);
#4448=ORIENTED_EDGE('',*,*,#3316,.T.);
#4449=ORIENTED_EDGE('',*,*,#3312,.F.);
#4450=ORIENTED_EDGE('',*,*,#3317,.T.);
#4451=ORIENTED_EDGE('',*,*,#3318,.T.);
#4452=ORIENTED_EDGE('',*,*,#3319,.T.);
#4453=ORIENTED_EDGE('',*,*,#3315,.F.);
#4454=ORIENTED_EDGE('',*,*,#3320,.T.);
#4455=ORIENTED_EDGE('',*,*,#3321,.T.);
#4456=ORIENTED_EDGE('',*,*,#3322,.T.);
#4457=ORIENTED_EDGE('',*,*,#3318,.F.);
#4458=ORIENTED_EDGE('',*,*,#3323,.T.);
#4459=ORIENTED_EDGE('',*,*,#3310,.T.);
#4460=ORIENTED_EDGE('',*,*,#3324,.T.);
#4461=ORIENTED_EDGE('',*,*,#3321,.F.);
#4462=ORIENTED_EDGE('',*,*,#3323,.F.);
#4463=ORIENTED_EDGE('',*,*,#3320,.F.);
#4464=ORIENTED_EDGE('',*,*,#3317,.F.);
#4465=ORIENTED_EDGE('',*,*,#3314,.F.);
#4466=ORIENTED_EDGE('',*,*,#3311,.F.);
#4467=ORIENTED_EDGE('',*,*,#3307,.F.);
#4468=ORIENTED_EDGE('',*,*,#3324,.F.);
#4469=ORIENTED_EDGE('',*,*,#3309,.F.);
#4470=ORIENTED_EDGE('',*,*,#3313,.F.);
#4471=ORIENTED_EDGE('',*,*,#3316,.F.);
#4472=ORIENTED_EDGE('',*,*,#3319,.F.);
#4473=ORIENTED_EDGE('',*,*,#3322,.F.);
#4474=ORIENTED_EDGE('',*,*,#3325,.F.);
#4475=ORIENTED_EDGE('',*,*,#3326,.F.);
#4476=ORIENTED_EDGE('',*,*,#3327,.F.);
#4477=ORIENTED_EDGE('',*,*,#3328,.T.);
#4478=ORIENTED_EDGE('',*,*,#3326,.T.);
#4479=ORIENTED_EDGE('',*,*,#3328,.F.);
#4480=ORIENTED_EDGE('',*,*,#3329,.F.);
#4481=ORIENTED_EDGE('',*,*,#3330,.T.);
#4482=ORIENTED_EDGE('',*,*,#3327,.T.);
#4483=ORIENTED_EDGE('',*,*,#3330,.F.);
#4484=ORIENTED_EDGE('',*,*,#3331,.F.);
#4485=ORIENTED_EDGE('',*,*,#3332,.T.);
#4486=ORIENTED_EDGE('',*,*,#3329,.T.);
#4487=ORIENTED_EDGE('',*,*,#3332,.F.);
#4488=ORIENTED_EDGE('',*,*,#3331,.T.);
#4489=ORIENTED_EDGE('',*,*,#3333,.F.);
#4490=ORIENTED_EDGE('',*,*,#3334,.F.);
#4491=ORIENTED_EDGE('',*,*,#3335,.T.);
#4492=ORIENTED_EDGE('',*,*,#3333,.T.);
#4493=ORIENTED_EDGE('',*,*,#3335,.F.);
#4494=ORIENTED_EDGE('',*,*,#3325,.T.);
#4495=ORIENTED_EDGE('',*,*,#3336,.T.);
#4496=ORIENTED_EDGE('',*,*,#3334,.T.);
#4497=ORIENTED_EDGE('',*,*,#3336,.F.);
#4498=ORIENTED_EDGE('',*,*,#3337,.F.);
#4499=ORIENTED_EDGE('',*,*,#3338,.T.);
#4500=ORIENTED_EDGE('',*,*,#3339,.F.);
#4501=ORIENTED_EDGE('',*,*,#3338,.F.);
#4502=ORIENTED_EDGE('',*,*,#3340,.F.);
#4503=ORIENTED_EDGE('',*,*,#3341,.T.);
#4504=ORIENTED_EDGE('',*,*,#3342,.F.);
#4505=ORIENTED_EDGE('',*,*,#3341,.F.);
#4506=ORIENTED_EDGE('',*,*,#3343,.F.);
#4507=ORIENTED_EDGE('',*,*,#3344,.F.);
#4508=ORIENTED_EDGE('',*,*,#3345,.F.);
#4509=ORIENTED_EDGE('',*,*,#3346,.T.);
#4510=ORIENTED_EDGE('',*,*,#3343,.T.);
#4511=ORIENTED_EDGE('',*,*,#3347,.T.);
#4512=ORIENTED_EDGE('',*,*,#3348,.F.);
#4513=ORIENTED_EDGE('',*,*,#3349,.F.);
#4514=ORIENTED_EDGE('',*,*,#3346,.F.);
#4515=ORIENTED_EDGE('',*,*,#3350,.F.);
#4516=ORIENTED_EDGE('',*,*,#3351,.F.);
#4517=ORIENTED_EDGE('',*,*,#3347,.F.);
#4518=ORIENTED_EDGE('',*,*,#3337,.T.);
#4519=ORIENTED_EDGE('',*,*,#3340,.T.);
#4520=ORIENTED_EDGE('',*,*,#3345,.T.);
#4521=ORIENTED_EDGE('',*,*,#3352,.F.);
#4522=ORIENTED_EDGE('',*,*,#3353,.F.);
#4523=ORIENTED_EDGE('',*,*,#3350,.T.);
#4524=ORIENTED_EDGE('',*,*,#3348,.T.);
#4525=ORIENTED_EDGE('',*,*,#3351,.T.);
#4526=ORIENTED_EDGE('',*,*,#3353,.T.);
#4527=ORIENTED_EDGE('',*,*,#3354,.F.);
#4528=ORIENTED_EDGE('',*,*,#3349,.T.);
#4529=ORIENTED_EDGE('',*,*,#3354,.T.);
#4530=ORIENTED_EDGE('',*,*,#3352,.T.);
#4531=ORIENTED_EDGE('',*,*,#3344,.T.);
#4532=ORIENTED_EDGE('',*,*,#3339,.T.);
#4533=ORIENTED_EDGE('',*,*,#3342,.T.);
#4534=ORIENTED_EDGE('',*,*,#3355,.F.);
#4535=ORIENTED_EDGE('',*,*,#3356,.T.);
#4536=ORIENTED_EDGE('',*,*,#3357,.F.);
#4537=ORIENTED_EDGE('',*,*,#3356,.F.);
#4538=ORIENTED_EDGE('',*,*,#3355,.T.);
#4539=ORIENTED_EDGE('',*,*,#3358,.F.);
#4540=ORIENTED_EDGE('',*,*,#3359,.T.);
#4541=ORIENTED_EDGE('',*,*,#3360,.F.);
#4542=ORIENTED_EDGE('',*,*,#3359,.F.);
#4543=ORIENTED_EDGE('',*,*,#3361,.F.);
#4544=ORIENTED_EDGE('',*,*,#3362,.T.);
#4545=ORIENTED_EDGE('',*,*,#3363,.F.);
#4546=ORIENTED_EDGE('',*,*,#3362,.F.);
#4547=ORIENTED_EDGE('',*,*,#3364,.F.);
#4548=ORIENTED_EDGE('',*,*,#3365,.F.);
#4549=ORIENTED_EDGE('',*,*,#3366,.F.);
#4550=ORIENTED_EDGE('',*,*,#3367,.T.);
#4551=ORIENTED_EDGE('',*,*,#3368,.T.);
#4552=ORIENTED_EDGE('',*,*,#3369,.T.);
#4553=ORIENTED_EDGE('',*,*,#3370,.T.);
#4554=ORIENTED_EDGE('',*,*,#3371,.T.);
#4555=ORIENTED_EDGE('',*,*,#3363,.T.);
#4556=ORIENTED_EDGE('',*,*,#3372,.F.);
#4557=ORIENTED_EDGE('',*,*,#3373,.T.);
#4558=ORIENTED_EDGE('',*,*,#3368,.F.);
#4559=ORIENTED_EDGE('',*,*,#3374,.F.);
#4560=ORIENTED_EDGE('',*,*,#3375,.F.);
#4561=ORIENTED_EDGE('',*,*,#3376,.T.);
#4562=ORIENTED_EDGE('',*,*,#3377,.F.);
#4563=ORIENTED_EDGE('',*,*,#3365,.T.);
#4564=ORIENTED_EDGE('',*,*,#3378,.T.);
#4565=ORIENTED_EDGE('',*,*,#3379,.T.);
#4566=ORIENTED_EDGE('',*,*,#3375,.T.);
#4567=ORIENTED_EDGE('',*,*,#3380,.T.);
#4568=ORIENTED_EDGE('',*,*,#3358,.T.);
#4569=ORIENTED_EDGE('',*,*,#3381,.F.);
#4570=ORIENTED_EDGE('',*,*,#3382,.T.);
#4571=ORIENTED_EDGE('',*,*,#3369,.F.);
#4572=ORIENTED_EDGE('',*,*,#3373,.F.);
#4573=ORIENTED_EDGE('',*,*,#3374,.T.);
#4574=ORIENTED_EDGE('',*,*,#3371,.F.);
#4575=ORIENTED_EDGE('',*,*,#3383,.F.);
#4576=ORIENTED_EDGE('',*,*,#3380,.F.);
#4577=ORIENTED_EDGE('',*,*,#3384,.F.);
#4578=ORIENTED_EDGE('',*,*,#3370,.F.);
#4579=ORIENTED_EDGE('',*,*,#3382,.F.);
#4580=ORIENTED_EDGE('',*,*,#3385,.F.);
#4581=ORIENTED_EDGE('',*,*,#3367,.F.);
#4582=ORIENTED_EDGE('',*,*,#3386,.F.);
#4583=ORIENTED_EDGE('',*,*,#3387,.F.);
#4584=ORIENTED_EDGE('',*,*,#3378,.F.);
#4585=ORIENTED_EDGE('',*,*,#3383,.T.);
#4586=ORIENTED_EDGE('',*,*,#3364,.T.);
#4587=ORIENTED_EDGE('',*,*,#3385,.T.);
#4588=ORIENTED_EDGE('',*,*,#3381,.T.);
#4589=ORIENTED_EDGE('',*,*,#3372,.T.);
#4590=ORIENTED_EDGE('',*,*,#3361,.T.);
#4591=ORIENTED_EDGE('',*,*,#3379,.F.);
#4592=ORIENTED_EDGE('',*,*,#3387,.T.);
#4593=ORIENTED_EDGE('',*,*,#3388,.F.);
#4594=ORIENTED_EDGE('',*,*,#3376,.F.);
#4595=ORIENTED_EDGE('',*,*,#3366,.T.);
#4596=ORIENTED_EDGE('',*,*,#3377,.T.);
#4597=ORIENTED_EDGE('',*,*,#3388,.T.);
#4598=ORIENTED_EDGE('',*,*,#3386,.T.);
#4599=ORIENTED_EDGE('',*,*,#3360,.T.);
#4600=ORIENTED_EDGE('',*,*,#3389,.F.);
#4601=ORIENTED_EDGE('',*,*,#3390,.T.);
#4602=ORIENTED_EDGE('',*,*,#3384,.T.);
#4603=ORIENTED_EDGE('',*,*,#3390,.F.);
#4604=ORIENTED_EDGE('',*,*,#3389,.T.);
#4605=ORIENTED_EDGE('',*,*,#3357,.T.);
#4606=ORIENTED_EDGE('',*,*,#3391,.F.);
#4607=ORIENTED_EDGE('',*,*,#3392,.T.);
#4608=ORIENTED_EDGE('',*,*,#3393,.F.);
#4609=ORIENTED_EDGE('',*,*,#3392,.F.);
#4610=ORIENTED_EDGE('',*,*,#3394,.F.);
#4611=ORIENTED_EDGE('',*,*,#3395,.T.);
#4612=ORIENTED_EDGE('',*,*,#3391,.T.);
#4613=ORIENTED_EDGE('',*,*,#3395,.F.);
#4614=ORIENTED_EDGE('',*,*,#3394,.T.);
#4615=ORIENTED_EDGE('',*,*,#3396,.F.);
#4616=ORIENTED_EDGE('',*,*,#3397,.T.);
#4617=ORIENTED_EDGE('',*,*,#3398,.F.);
#4618=ORIENTED_EDGE('',*,*,#3399,.F.);
#4619=ORIENTED_EDGE('',*,*,#3400,.F.);
#4620=ORIENTED_EDGE('',*,*,#3401,.F.);
#4621=ORIENTED_EDGE('',*,*,#3402,.F.);
#4622=ORIENTED_EDGE('',*,*,#3403,.F.);
#4623=ORIENTED_EDGE('',*,*,#3397,.F.);
#4624=ORIENTED_EDGE('',*,*,#3402,.T.);
#4625=ORIENTED_EDGE('',*,*,#3404,.F.);
#4626=ORIENTED_EDGE('',*,*,#3405,.T.);
#4627=ORIENTED_EDGE('',*,*,#3406,.T.);
#4628=ORIENTED_EDGE('',*,*,#3401,.T.);
#4629=ORIENTED_EDGE('',*,*,#3407,.F.);
#4630=ORIENTED_EDGE('',*,*,#3408,.T.);
#4631=ORIENTED_EDGE('',*,*,#3404,.T.);
#4632=ORIENTED_EDGE('',*,*,#3400,.T.);
#4633=ORIENTED_EDGE('',*,*,#3409,.F.);
#4634=ORIENTED_EDGE('',*,*,#3410,.T.);
#4635=ORIENTED_EDGE('',*,*,#3407,.T.);
#4636=ORIENTED_EDGE('',*,*,#3399,.T.);
#4637=ORIENTED_EDGE('',*,*,#3411,.F.);
#4638=ORIENTED_EDGE('',*,*,#3412,.T.);
#4639=ORIENTED_EDGE('',*,*,#3409,.T.);
#4640=ORIENTED_EDGE('',*,*,#3398,.T.);
#4641=ORIENTED_EDGE('',*,*,#3413,.F.);
#4642=ORIENTED_EDGE('',*,*,#3414,.T.);
#4643=ORIENTED_EDGE('',*,*,#3411,.T.);
#4644=ORIENTED_EDGE('',*,*,#3403,.T.);
#4645=ORIENTED_EDGE('',*,*,#3406,.F.);
#4646=ORIENTED_EDGE('',*,*,#3415,.T.);
#4647=ORIENTED_EDGE('',*,*,#3413,.T.);
#4648=ORIENTED_EDGE('',*,*,#3396,.T.);
#4649=ORIENTED_EDGE('',*,*,#3410,.F.);
#4650=ORIENTED_EDGE('',*,*,#3412,.F.);
#4651=ORIENTED_EDGE('',*,*,#3414,.F.);
#4652=ORIENTED_EDGE('',*,*,#3415,.F.);
#4653=ORIENTED_EDGE('',*,*,#3405,.F.);
#4654=ORIENTED_EDGE('',*,*,#3408,.F.);
#4655=ORIENTED_EDGE('',*,*,#3393,.T.);
#4656=ORIENTED_EDGE('',*,*,#3416,.F.);
#4657=ORIENTED_EDGE('',*,*,#3417,.F.);
#4658=ORIENTED_EDGE('',*,*,#3418,.T.);
#4659=ORIENTED_EDGE('',*,*,#3419,.F.);
#4660=ORIENTED_EDGE('',*,*,#3418,.F.);
#4661=ORIENTED_EDGE('',*,*,#3420,.F.);
#4662=ORIENTED_EDGE('',*,*,#3421,.F.);
#4663=ORIENTED_EDGE('',*,*,#3422,.F.);
#4664=ORIENTED_EDGE('',*,*,#3423,.F.);
#4665=ORIENTED_EDGE('',*,*,#3424,.F.);
#4666=ORIENTED_EDGE('',*,*,#3425,.T.);
#4667=ORIENTED_EDGE('',*,*,#3426,.F.);
#4668=ORIENTED_EDGE('',*,*,#3427,.F.);
#4669=ORIENTED_EDGE('',*,*,#3428,.F.);
#4670=ORIENTED_EDGE('',*,*,#3429,.F.);
#4671=ORIENTED_EDGE('',*,*,#3430,.F.);
#4672=ORIENTED_EDGE('',*,*,#3431,.F.);
#4673=ORIENTED_EDGE('',*,*,#3425,.F.);
#4674=ORIENTED_EDGE('',*,*,#3421,.T.);
#4675=ORIENTED_EDGE('',*,*,#3432,.T.);
#4676=ORIENTED_EDGE('',*,*,#3430,.T.);
#4677=ORIENTED_EDGE('',*,*,#3433,.F.);
#4678=ORIENTED_EDGE('',*,*,#3420,.T.);
#4679=ORIENTED_EDGE('',*,*,#3434,.T.);
#4680=ORIENTED_EDGE('',*,*,#3431,.T.);
#4681=ORIENTED_EDGE('',*,*,#3432,.F.);
#4682=ORIENTED_EDGE('',*,*,#3417,.T.);
#4683=ORIENTED_EDGE('',*,*,#3435,.T.);
#4684=ORIENTED_EDGE('',*,*,#3426,.T.);
#4685=ORIENTED_EDGE('',*,*,#3434,.F.);
#4686=ORIENTED_EDGE('',*,*,#3436,.F.);
#4687=ORIENTED_EDGE('',*,*,#3437,.T.);
#4688=ORIENTED_EDGE('',*,*,#3438,.T.);
#4689=ORIENTED_EDGE('',*,*,#3437,.F.);
#4690=ORIENTED_EDGE('',*,*,#3416,.T.);
#4691=ORIENTED_EDGE('',*,*,#3439,.T.);
#4692=ORIENTED_EDGE('',*,*,#3427,.T.);
#4693=ORIENTED_EDGE('',*,*,#3435,.F.);
#4694=ORIENTED_EDGE('',*,*,#3422,.T.);
#4695=ORIENTED_EDGE('',*,*,#3433,.T.);
#4696=ORIENTED_EDGE('',*,*,#3429,.T.);
#4697=ORIENTED_EDGE('',*,*,#3440,.F.);
#4698=ORIENTED_EDGE('',*,*,#3423,.T.);
#4699=ORIENTED_EDGE('',*,*,#3440,.T.);
#4700=ORIENTED_EDGE('',*,*,#3428,.T.);
#4701=ORIENTED_EDGE('',*,*,#3439,.F.);
#4702=ORIENTED_EDGE('',*,*,#3424,.T.);
#4703=ORIENTED_EDGE('',*,*,#3436,.T.);
#4704=ORIENTED_EDGE('',*,*,#3419,.T.);
#4705=ORIENTED_EDGE('',*,*,#3438,.F.);
#4706=ORIENTED_EDGE('',*,*,#3441,.F.);
#4707=ORIENTED_EDGE('',*,*,#3442,.T.);
#4708=ORIENTED_EDGE('',*,*,#3443,.T.);
#4709=ORIENTED_EDGE('',*,*,#3442,.F.);
#4710=ORIENTED_EDGE('',*,*,#3441,.T.);
#4711=ORIENTED_EDGE('',*,*,#3443,.F.);
#4712=ORIENTED_EDGE('',*,*,#3444,.F.);
#4713=ORIENTED_EDGE('',*,*,#3445,.T.);
#4714=ORIENTED_EDGE('',*,*,#3446,.F.);
#4715=ORIENTED_EDGE('',*,*,#3445,.F.);
#4716=ORIENTED_EDGE('',*,*,#3447,.F.);
#4717=ORIENTED_EDGE('',*,*,#3448,.F.);
#4718=ORIENTED_EDGE('',*,*,#3449,.F.);
#4719=ORIENTED_EDGE('',*,*,#3450,.F.);
#4720=ORIENTED_EDGE('',*,*,#3451,.T.);
#4721=ORIENTED_EDGE('',*,*,#3449,.T.);
#4722=ORIENTED_EDGE('',*,*,#3451,.F.);
#4723=ORIENTED_EDGE('',*,*,#3452,.F.);
#4724=ORIENTED_EDGE('',*,*,#3453,.T.);
#4725=ORIENTED_EDGE('',*,*,#3450,.T.);
#4726=ORIENTED_EDGE('',*,*,#3453,.F.);
#4727=ORIENTED_EDGE('',*,*,#3452,.T.);
#4728=ORIENTED_EDGE('',*,*,#3454,.F.);
#4729=ORIENTED_EDGE('',*,*,#3455,.F.);
#4730=ORIENTED_EDGE('',*,*,#3456,.T.);
#4731=ORIENTED_EDGE('',*,*,#3448,.T.);
#4732=ORIENTED_EDGE('',*,*,#3457,.T.);
#4733=ORIENTED_EDGE('',*,*,#3454,.T.);
#4734=ORIENTED_EDGE('',*,*,#3457,.F.);
#4735=ORIENTED_EDGE('',*,*,#3447,.T.);
#4736=ORIENTED_EDGE('',*,*,#3444,.T.);
#4737=ORIENTED_EDGE('',*,*,#3456,.F.);
#4738=ORIENTED_EDGE('',*,*,#3446,.T.);
#4739=ORIENTED_EDGE('',*,*,#3458,.F.);
#4740=ORIENTED_EDGE('',*,*,#3459,.T.);
#4741=ORIENTED_EDGE('',*,*,#3455,.T.);
#4742=ORIENTED_EDGE('',*,*,#3459,.F.);
#4743=ORIENTED_EDGE('',*,*,#3458,.T.);
#4744=ORIENTED_EDGE('',*,*,#3460,.F.);
#4745=ORIENTED_EDGE('',*,*,#3461,.T.);
#4746=ORIENTED_EDGE('',*,*,#3462,.T.);
#4747=ORIENTED_EDGE('',*,*,#3461,.F.);
#4748=ORIENTED_EDGE('',*,*,#3463,.F.);
#4749=ORIENTED_EDGE('',*,*,#3464,.T.);
#4750=ORIENTED_EDGE('',*,*,#3465,.T.);
#4751=ORIENTED_EDGE('',*,*,#3464,.F.);
#4752=ORIENTED_EDGE('',*,*,#3463,.T.);
#4753=ORIENTED_EDGE('',*,*,#3460,.T.);
#4754=ORIENTED_EDGE('',*,*,#3465,.F.);
#4755=ORIENTED_EDGE('',*,*,#3462,.F.);
#4756=ORIENTED_EDGE('',*,*,#3466,.F.);
#4757=ORIENTED_EDGE('',*,*,#3467,.T.);
#4758=ORIENTED_EDGE('',*,*,#3468,.T.);
#4759=ORIENTED_EDGE('',*,*,#3467,.F.);
#4760=ORIENTED_EDGE('',*,*,#3469,.F.);
#4761=ORIENTED_EDGE('',*,*,#3470,.T.);
#4762=ORIENTED_EDGE('',*,*,#3471,.T.);
#4763=ORIENTED_EDGE('',*,*,#3470,.F.);
#4764=ORIENTED_EDGE('',*,*,#3469,.T.);
#4765=ORIENTED_EDGE('',*,*,#3466,.T.);
#4766=ORIENTED_EDGE('',*,*,#3471,.F.);
#4767=ORIENTED_EDGE('',*,*,#3468,.F.);
#4768=ORIENTED_EDGE('',*,*,#3472,.F.);
#4769=ORIENTED_EDGE('',*,*,#3473,.T.);
#4770=ORIENTED_EDGE('',*,*,#3472,.T.);
#4771=ORIENTED_EDGE('',*,*,#3473,.F.);
#4772=ORIENTED_EDGE('',*,*,#3474,.F.);
#4773=ORIENTED_EDGE('',*,*,#3475,.F.);
#4774=ORIENTED_EDGE('',*,*,#3476,.T.);
#4775=ORIENTED_EDGE('',*,*,#3477,.F.);
#4776=ORIENTED_EDGE('',*,*,#3477,.T.);
#4777=ORIENTED_EDGE('',*,*,#3478,.T.);
#4778=ORIENTED_EDGE('',*,*,#3479,.F.);
#4779=ORIENTED_EDGE('',*,*,#3480,.F.);
#4780=ORIENTED_EDGE('',*,*,#3476,.F.);
#4781=ORIENTED_EDGE('',*,*,#3480,.T.);
#4782=ORIENTED_EDGE('',*,*,#3481,.F.);
#4783=ORIENTED_EDGE('',*,*,#3482,.T.);
#4784=ORIENTED_EDGE('',*,*,#3475,.T.);
#4785=ORIENTED_EDGE('',*,*,#3474,.T.);
#4786=ORIENTED_EDGE('',*,*,#3482,.F.);
#4787=ORIENTED_EDGE('',*,*,#3483,.F.);
#4788=ORIENTED_EDGE('',*,*,#3478,.F.);
#4789=ORIENTED_EDGE('',*,*,#3483,.T.);
#4790=ORIENTED_EDGE('',*,*,#3481,.T.);
#4791=ORIENTED_EDGE('',*,*,#3479,.T.);
#4792=CYLINDRICAL_SURFACE('',#5464,0.3);
#4793=CYLINDRICAL_SURFACE('',#5479,0.275);
#4794=CYLINDRICAL_SURFACE('',#5481,0.275);
#4795=CYLINDRICAL_SURFACE('',#5483,0.51);
#4796=CYLINDRICAL_SURFACE('',#5491,0.31);
#4797=CYLINDRICAL_SURFACE('',#5494,0.31);
#4798=CYLINDRICAL_SURFACE('',#5512,0.6);
#4799=CYLINDRICAL_SURFACE('',#5519,0.33);
#4800=CYLINDRICAL_SURFACE('',#5521,0.33);
#4801=CYLINDRICAL_SURFACE('',#5524,0.210000000000001);
#4802=CYLINDRICAL_SURFACE('',#5532,0.21);
#4803=CYLINDRICAL_SURFACE('',#5550,0.265);
#4804=CYLINDRICAL_SURFACE('',#5554,0.5);
#4805=CYLINDRICAL_SURFACE('',#5572,0.425);
#4806=CYLINDRICAL_SURFACE('',#5580,0.24505);
#4807=CYLINDRICAL_SURFACE('',#5582,0.3);
#4808=CYLINDRICAL_SURFACE('',#5585,0.3);
#4809=CYLINDRICAL_SURFACE('',#5588,0.33);
#4810=CYLINDRICAL_SURFACE('',#5591,0.33);
#4811=CYLINDRICAL_SURFACE('',#5594,0.33);
#4812=CYLINDRICAL_SURFACE('',#5597,0.33);
#4813=CYLINDRICAL_SURFACE('',#5600,0.33);
#4814=CYLINDRICAL_SURFACE('',#5603,0.33);
#4815=CYLINDRICAL_SURFACE('',#5606,0.34);
#4816=CYLINDRICAL_SURFACE('',#5609,0.34);
#4817=CYLINDRICAL_SURFACE('',#5612,0.34);
#4818=CYLINDRICAL_SURFACE('',#5615,0.34);
#4819=CYLINDRICAL_SURFACE('',#5618,0.34);
#4820=CYLINDRICAL_SURFACE('',#5621,0.34);
#4821=CYLINDRICAL_SURFACE('',#5624,0.34);
#4822=CYLINDRICAL_SURFACE('',#5627,0.34);
#4823=CYLINDRICAL_SURFACE('',#5630,0.34);
#4824=CYLINDRICAL_SURFACE('',#5633,0.34);
#4825=CYLINDRICAL_SURFACE('',#5636,0.34);
#4826=CYLINDRICAL_SURFACE('',#5639,0.34);
#4827=CYLINDRICAL_SURFACE('',#5642,0.34);
#4828=CYLINDRICAL_SURFACE('',#5645,0.34);
#4829=CYLINDRICAL_SURFACE('',#5648,0.34);
#4830=CYLINDRICAL_SURFACE('',#5651,0.34);
#4831=CYLINDRICAL_SURFACE('',#5654,0.34);
#4832=CYLINDRICAL_SURFACE('',#5657,0.34);
#4833=CYLINDRICAL_SURFACE('',#5660,0.34);
#4834=CYLINDRICAL_SURFACE('',#5663,0.34);
#4835=CYLINDRICAL_SURFACE('',#5673,0.425);
#4836=CYLINDRICAL_SURFACE('',#5676,0.425);
#4837=CYLINDRICAL_SURFACE('',#5686,0.2942);
#4838=CYLINDRICAL_SURFACE('',#5710,0.25175);
#4839=CYLINDRICAL_SURFACE('',#5719,0.4);
#4840=CYLINDRICAL_SURFACE('',#5723,0.8);
#4841=CYLINDRICAL_SURFACE('',#5731,0.3);
#4842=CYLINDRICAL_SURFACE('',#5740,0.3);
#4843=CYLINDRICAL_SURFACE('',#5769,0.65);
#4844=CYLINDRICAL_SURFACE('',#5777,0.3933);
#4845=CYLINDRICAL_SURFACE('',#5780,0.275);
#4846=CYLINDRICAL_SURFACE('',#5783,0.31);
#4847=CYLINDRICAL_SURFACE('',#5786,0.7);
#4848=CYLINDRICAL_SURFACE('',#5795,0.31);
#4849=CYLINDRICAL_SURFACE('',#5798,0.31);
#4850=CYLINDRICAL_SURFACE('',#5811,0.6);
#4851=CYLINDRICAL_SURFACE('',#5823,0.21);
#4852=CYLINDRICAL_SURFACE('',#5827,0.7);
#4853=CYLINDRICAL_SURFACE('',#5847,0.425);
#4854=CYLINDRICAL_SURFACE('',#5855,0.24505);
#4855=CYLINDRICAL_SURFACE('',#5858,0.31);
#4856=CYLINDRICAL_SURFACE('',#5861,0.31);
#4857=CYLINDRICAL_SURFACE('',#5864,0.6);
#4858=CYLINDRICAL_SURFACE('',#5871,0.6);
#4859=CYLINDRICAL_SURFACE('',#5877,0.34);
#4860=CYLINDRICAL_SURFACE('',#5881,0.31);
#4861=CYLINDRICAL_SURFACE('',#5884,0.31);
#4862=CYLINDRICAL_SURFACE('',#5898,0.5);
#4863=CYLINDRICAL_SURFACE('',#5902,0.3933);
#4864=CYLINDRICAL_SURFACE('',#5926,0.338975);
#4865=CYLINDRICAL_SURFACE('',#5935,1.);
#4866=CYLINDRICAL_SURFACE('',#5941,0.08);
#4867=CYLINDRICAL_SURFACE('',#5946,0.5);
#4868=CYLINDRICAL_SURFACE('',#5950,0.3);
#4869=CYLINDRICAL_SURFACE('',#5956,0.32);
#4870=CYLINDRICAL_SURFACE('',#5959,0.6);
#4871=CYLINDRICAL_SURFACE('',#5965,0.31);
#4872=CYLINDRICAL_SURFACE('',#5968,0.5);
#4873=CYLINDRICAL_SURFACE('',#5980,0.08);
#4874=ADVANCED_FACE('',(#673),#4792,.T.);
#4875=ADVANCED_FACE('',(#674),#486,.F.);
#4876=ADVANCED_FACE('',(#675),#487,.T.);
#4877=ADVANCED_FACE('',(#676),#488,.T.);
#4878=ADVANCED_FACE('',(#677),#489,.T.);
#4879=ADVANCED_FACE('',(#678),#490,.T.);
#4880=ADVANCED_FACE('',(#679),#491,.T.);
#4881=ADVANCED_FACE('',(#680),#492,.F.);
#4882=ADVANCED_FACE('',(#681,#366,#367,#368,#369,#370),#493,.T.);
#4883=ADVANCED_FACE('',(#682),#4793,.F.);
#4884=ADVANCED_FACE('',(#683),#4794,.F.);
#4885=ADVANCED_FACE('',(#684),#4795,.F.);
#4886=ADVANCED_FACE('',(#685),#494,.F.);
#4887=ADVANCED_FACE('',(#686,#371),#495,.T.);
#4888=ADVANCED_FACE('',(#687,#372),#496,.T.);
#4889=ADVANCED_FACE('',(#688),#497,.T.);
#4890=ADVANCED_FACE('',(#689),#498,.T.);
#4891=ADVANCED_FACE('',(#690),#4796,.F.);
#4892=ADVANCED_FACE('',(#691),#4797,.F.);
#4893=ADVANCED_FACE('',(#692,#373),#499,.F.);
#4894=ADVANCED_FACE('',(#693),#500,.T.);
#4895=ADVANCED_FACE('',(#694),#501,.T.);
#4896=ADVANCED_FACE('',(#695),#502,.T.);
#4897=ADVANCED_FACE('',(#696,#374),#503,.T.);
#4898=ADVANCED_FACE('',(#697,#375),#504,.F.);
#4899=ADVANCED_FACE('',(#698),#505,.T.);
#4900=ADVANCED_FACE('',(#699),#506,.T.);
#4901=ADVANCED_FACE('',(#700),#507,.T.);
#4902=ADVANCED_FACE('',(#701,#376),#508,.T.);
#4903=ADVANCED_FACE('',(#702),#509,.T.);
#4904=ADVANCED_FACE('',(#703),#510,.T.);
#4905=ADVANCED_FACE('',(#704),#511,.T.);
#4906=ADVANCED_FACE('',(#705,#377,#378),#512,.F.);
#4907=ADVANCED_FACE('',(#706),#4798,.F.);
#4908=ADVANCED_FACE('',(#707),#513,.T.);
#4909=ADVANCED_FACE('',(#708,#379,#380),#514,.F.);
#4910=ADVANCED_FACE('',(#709),#4799,.F.);
#4911=ADVANCED_FACE('',(#710),#4800,.F.);
#4912=ADVANCED_FACE('',(#711),#515,.T.);
#4913=ADVANCED_FACE('',(#712),#4801,.F.);
#4914=ADVANCED_FACE('',(#713),#516,.T.);
#4915=ADVANCED_FACE('',(#714),#517,.T.);
#4916=ADVANCED_FACE('',(#715),#518,.T.);
#4917=ADVANCED_FACE('',(#716,#381),#519,.T.);
#4918=ADVANCED_FACE('',(#717),#520,.T.);
#4919=ADVANCED_FACE('',(#718),#4802,.F.);
#4920=ADVANCED_FACE('',(#719),#521,.T.);
#4921=ADVANCED_FACE('',(#720),#522,.T.);
#4922=ADVANCED_FACE('',(#721),#523,.T.);
#4923=ADVANCED_FACE('',(#722,#382),#524,.T.);
#4924=ADVANCED_FACE('',(#723),#525,.T.);
#4925=ADVANCED_FACE('',(#724),#526,.T.);
#4926=ADVANCED_FACE('',(#725,#383,#384),#527,.T.);
#4927=ADVANCED_FACE('',(#726),#528,.T.);
#4928=ADVANCED_FACE('',(#727),#529,.T.);
#4929=ADVANCED_FACE('',(#728),#530,.T.);
#4930=ADVANCED_FACE('',(#729),#531,.F.);
#4931=ADVANCED_FACE('',(#730),#250,.F.);
#4932=ADVANCED_FACE('',(#731),#4803,.F.);
#4933=ADVANCED_FACE('',(#732,#385),#532,.T.);
#4934=ADVANCED_FACE('',(#733),#4804,.T.);
#4935=ADVANCED_FACE('',(#734,#386),#533,.F.);
#4936=ADVANCED_FACE('',(#735),#534,.F.);
#4937=ADVANCED_FACE('',(#736),#535,.F.);
#4938=ADVANCED_FACE('',(#737),#536,.F.);
#4939=ADVANCED_FACE('',(#738),#537,.F.);
#4940=ADVANCED_FACE('',(#739),#538,.F.);
#4941=ADVANCED_FACE('',(#740),#539,.F.);
#4942=ADVANCED_FACE('',(#741),#540,.F.);
#4943=ADVANCED_FACE('',(#742),#541,.F.);
#4944=ADVANCED_FACE('',(#743),#542,.F.);
#4945=ADVANCED_FACE('',(#744),#543,.T.);
#4946=ADVANCED_FACE('',(#745),#251,.T.);
#4947=ADVANCED_FACE('',(#746),#4805,.T.);
#4948=ADVANCED_FACE('',(#747),#252,.T.);
#4949=ADVANCED_FACE('',(#748,#387),#544,.T.);
#4950=ADVANCED_FACE('',(#749),#253,.T.);
#4951=ADVANCED_FACE('',(#750),#4806,.T.);
#4952=ADVANCED_FACE('',(#751),#4807,.F.);
#4953=ADVANCED_FACE('',(#752),#4808,.F.);
#4954=ADVANCED_FACE('',(#753),#4809,.F.);
#4955=ADVANCED_FACE('',(#754),#4810,.F.);
#4956=ADVANCED_FACE('',(#755),#4811,.F.);
#4957=ADVANCED_FACE('',(#756),#4812,.F.);
#4958=ADVANCED_FACE('',(#757),#4813,.F.);
#4959=ADVANCED_FACE('',(#758),#4814,.F.);
#4960=ADVANCED_FACE('',(#759),#4815,.F.);
#4961=ADVANCED_FACE('',(#760),#4816,.F.);
#4962=ADVANCED_FACE('',(#761),#4817,.F.);
#4963=ADVANCED_FACE('',(#762),#4818,.F.);
#4964=ADVANCED_FACE('',(#763),#4819,.F.);
#4965=ADVANCED_FACE('',(#764),#4820,.F.);
#4966=ADVANCED_FACE('',(#765),#4821,.F.);
#4967=ADVANCED_FACE('',(#766),#4822,.F.);
#4968=ADVANCED_FACE('',(#767),#4823,.F.);
#4969=ADVANCED_FACE('',(#768),#4824,.F.);
#4970=ADVANCED_FACE('',(#769),#4825,.F.);
#4971=ADVANCED_FACE('',(#770),#4826,.F.);
#4972=ADVANCED_FACE('',(#771),#4827,.F.);
#4973=ADVANCED_FACE('',(#772),#4828,.F.);
#4974=ADVANCED_FACE('',(#773),#4829,.F.);
#4975=ADVANCED_FACE('',(#774),#4830,.F.);
#4976=ADVANCED_FACE('',(#775),#4831,.F.);
#4977=ADVANCED_FACE('',(#776),#4832,.F.);
#4978=ADVANCED_FACE('',(#777),#4833,.F.);
#4979=ADVANCED_FACE('',(#778),#4834,.F.);
#4980=ADVANCED_FACE('',(#779),#545,.T.);
#4981=ADVANCED_FACE('',(#780,#388,#389,#390,#391,#392,#393,#394,#395,#396,
#397,#398,#399,#400,#401,#402,#403,#404,#405,#406,#407,#408,#409,#410,#411,
#412,#413,#414,#415),#546,.T.);
#4982=ADVANCED_FACE('',(#781),#547,.T.);
#4983=ADVANCED_FACE('',(#782,#416,#417,#418,#419,#420,#421,#422,#423,#424,
#425,#426,#427,#428,#429,#430,#431,#432,#433,#434,#435,#436,#437,#438,#439,
#440,#441,#442,#443),#548,.T.);
#4984=ADVANCED_FACE('',(#783),#549,.T.);
#4985=ADVANCED_FACE('',(#784),#550,.F.);
#4986=ADVANCED_FACE('',(#785),#4835,.F.);
#4987=ADVANCED_FACE('',(#786),#4836,.F.);
#4988=ADVANCED_FACE('',(#787),#551,.T.);
#4989=ADVANCED_FACE('',(#788,#444,#445),#552,.T.);
#4990=ADVANCED_FACE('',(#789),#553,.T.);
#4991=ADVANCED_FACE('',(#790,#446,#447),#554,.T.);
#4992=ADVANCED_FACE('',(#791),#555,.T.);
#4993=ADVANCED_FACE('',(#792),#556,.F.);
#4994=ADVANCED_FACE('',(#793),#4837,.T.);
#4995=ADVANCED_FACE('',(#794),#254,.T.);
#4996=ADVANCED_FACE('',(#795),#557,.T.);
#4997=ADVANCED_FACE('',(#796),#255,.T.);
#4998=ADVANCED_FACE('',(#797),#558,.T.);
#4999=ADVANCED_FACE('',(#798),#559,.T.);
#5000=ADVANCED_FACE('',(#799),#560,.T.);
#5001=ADVANCED_FACE('',(#800),#561,.T.);
#5002=ADVANCED_FACE('',(#801),#562,.T.);
#5003=ADVANCED_FACE('',(#802),#563,.T.);
#5004=ADVANCED_FACE('',(#803),#564,.T.);
#5005=ADVANCED_FACE('',(#804,#448),#565,.F.);
#5006=ADVANCED_FACE('',(#805),#256,.T.);
#5007=ADVANCED_FACE('',(#806),#257,.T.);
#5008=ADVANCED_FACE('',(#807),#566,.T.);
#5009=ADVANCED_FACE('',(#808),#567,.T.);
#5010=ADVANCED_FACE('',(#809),#568,.T.);
#5011=ADVANCED_FACE('',(#810),#4838,.F.);
#5012=ADVANCED_FACE('',(#811),#569,.T.);
#5013=ADVANCED_FACE('',(#812),#570,.T.);
#5014=ADVANCED_FACE('',(#813),#571,.T.);
#5015=ADVANCED_FACE('',(#814,#449),#572,.T.);
#5016=ADVANCED_FACE('',(#815,#450),#573,.F.);
#5017=ADVANCED_FACE('',(#816),#4839,.T.);
#5018=ADVANCED_FACE('',(#817),#574,.T.);
#5019=ADVANCED_FACE('',(#818),#4840,.T.);
#5020=ADVANCED_FACE('',(#819,#451),#575,.T.);
#5021=ADVANCED_FACE('',(#820),#576,.F.);
#5022=ADVANCED_FACE('',(#821),#202,.T.);
#5023=ADVANCED_FACE('',(#822),#4841,.T.);
#5024=ADVANCED_FACE('',(#823),#258,.T.);
#5025=ADVANCED_FACE('',(#824),#577,.T.);
#5026=ADVANCED_FACE('',(#825),#578,.F.);
#5027=ADVANCED_FACE('',(#826),#579,.T.);
#5028=ADVANCED_FACE('',(#827),#4842,.T.);
#5029=ADVANCED_FACE('',(#828),#259,.T.);
#5030=ADVANCED_FACE('',(#829),#580,.F.);
#5031=ADVANCED_FACE('',(#830),#581,.F.);
#5032=ADVANCED_FACE('',(#831),#582,.T.);
#5033=ADVANCED_FACE('',(#832),#203,.T.);
#5034=ADVANCED_FACE('',(#833),#260,.T.);
#5035=ADVANCED_FACE('',(#834),#583,.F.);
#5036=ADVANCED_FACE('',(#835),#584,.F.);
#5037=ADVANCED_FACE('',(#836),#585,.F.);
#5038=ADVANCED_FACE('',(#837),#586,.F.);
#5039=ADVANCED_FACE('',(#838),#587,.F.);
#5040=ADVANCED_FACE('',(#839),#588,.F.);
#5041=ADVANCED_FACE('',(#840),#589,.F.);
#5042=ADVANCED_FACE('',(#841),#590,.F.);
#5043=ADVANCED_FACE('',(#842),#591,.F.);
#5044=ADVANCED_FACE('',(#843),#592,.T.);
#5045=ADVANCED_FACE('',(#844),#261,.T.);
#5046=ADVANCED_FACE('',(#845),#4843,.T.);
#5047=ADVANCED_FACE('',(#846),#262,.T.);
#5048=ADVANCED_FACE('',(#847,#452),#593,.T.);
#5049=ADVANCED_FACE('',(#848),#263,.T.);
#5050=ADVANCED_FACE('',(#849),#4844,.T.);
#5051=ADVANCED_FACE('',(#850),#4845,.F.);
#5052=ADVANCED_FACE('',(#851),#4846,.F.);
#5053=ADVANCED_FACE('',(#852),#4847,.T.);
#5054=ADVANCED_FACE('',(#853,#453),#594,.F.);
#5055=ADVANCED_FACE('',(#854),#595,.T.);
#5056=ADVANCED_FACE('',(#855,#454),#596,.T.);
#5057=ADVANCED_FACE('',(#856),#597,.T.);
#5058=ADVANCED_FACE('',(#857),#4848,.F.);
#5059=ADVANCED_FACE('',(#858),#4849,.F.);
#5060=ADVANCED_FACE('',(#859),#598,.T.);
#5061=ADVANCED_FACE('',(#860,#455),#599,.T.);
#5062=ADVANCED_FACE('',(#861),#600,.T.);
#5063=ADVANCED_FACE('',(#862,#456),#601,.F.);
#5064=ADVANCED_FACE('',(#863),#602,.F.);
#5065=ADVANCED_FACE('',(#864),#603,.T.);
#5066=ADVANCED_FACE('',(#865),#604,.T.);
#5067=ADVANCED_FACE('',(#866),#605,.T.);
#5068=ADVANCED_FACE('',(#867,#457,#458),#4850,.T.);
#5069=ADVANCED_FACE('',(#868,#459),#606,.T.);
#5070=ADVANCED_FACE('',(#869,#460),#607,.F.);
#5071=ADVANCED_FACE('',(#870),#608,.T.);
#5072=ADVANCED_FACE('',(#871,#461),#609,.T.);
#5073=ADVANCED_FACE('',(#872,#462),#610,.T.);
#5074=ADVANCED_FACE('',(#873),#611,.T.);
#5075=ADVANCED_FACE('',(#874),#612,.T.);
#5076=ADVANCED_FACE('',(#875,#463),#613,.F.);
#5077=ADVANCED_FACE('',(#876),#4851,.F.);
#5078=ADVANCED_FACE('',(#877),#614,.T.);
#5079=ADVANCED_FACE('',(#878),#4852,.T.);
#5080=ADVANCED_FACE('',(#879,#464),#615,.T.);
#5081=ADVANCED_FACE('',(#880),#616,.F.);
#5082=ADVANCED_FACE('',(#881),#617,.F.);
#5083=ADVANCED_FACE('',(#882),#618,.F.);
#5084=ADVANCED_FACE('',(#883),#619,.F.);
#5085=ADVANCED_FACE('',(#884),#620,.F.);
#5086=ADVANCED_FACE('',(#885),#621,.F.);
#5087=ADVANCED_FACE('',(#886),#622,.F.);
#5088=ADVANCED_FACE('',(#887),#623,.F.);
#5089=ADVANCED_FACE('',(#888),#624,.F.);
#5090=ADVANCED_FACE('',(#889),#625,.F.);
#5091=ADVANCED_FACE('',(#890),#626,.T.);
#5092=ADVANCED_FACE('',(#891),#264,.T.);
#5093=ADVANCED_FACE('',(#892),#4853,.T.);
#5094=ADVANCED_FACE('',(#893),#265,.T.);
#5095=ADVANCED_FACE('',(#894,#465),#627,.T.);
#5096=ADVANCED_FACE('',(#895),#266,.T.);
#5097=ADVANCED_FACE('',(#896),#4854,.T.);
#5098=ADVANCED_FACE('',(#897),#4855,.F.);
#5099=ADVANCED_FACE('',(#898),#4856,.F.);
#5100=ADVANCED_FACE('',(#899),#4857,.T.);
#5101=ADVANCED_FACE('',(#900),#628,.T.);
#5102=ADVANCED_FACE('',(#901,#466,#467),#629,.F.);
#5103=ADVANCED_FACE('',(#902),#630,.T.);
#5104=ADVANCED_FACE('',(#903),#4858,.T.);
#5105=ADVANCED_FACE('',(#904,#468,#469),#631,.T.);
#5106=ADVANCED_FACE('',(#905),#4859,.F.);
#5107=ADVANCED_FACE('',(#906),#632,.T.);
#5108=ADVANCED_FACE('',(#907),#4860,.F.);
#5109=ADVANCED_FACE('',(#908),#4861,.F.);
#5110=ADVANCED_FACE('',(#909),#633,.T.);
#5111=ADVANCED_FACE('',(#910,#470),#634,.T.);
#5112=ADVANCED_FACE('',(#911),#635,.T.);
#5113=ADVANCED_FACE('',(#912,#471),#636,.F.);
#5114=ADVANCED_FACE('',(#913),#637,.T.);
#5115=ADVANCED_FACE('',(#914,#472),#638,.T.);
#5116=ADVANCED_FACE('',(#915),#639,.T.);
#5117=ADVANCED_FACE('',(#916,#473),#640,.F.);
#5118=ADVANCED_FACE('',(#917),#641,.T.);
#5119=ADVANCED_FACE('',(#918,#474),#642,.T.);
#5120=ADVANCED_FACE('',(#919),#4862,.T.);
#5121=ADVANCED_FACE('',(#920,#475),#643,.T.);
#5122=ADVANCED_FACE('',(#921),#4863,.T.);
#5123=ADVANCED_FACE('',(#922),#267,.T.);
#5124=ADVANCED_FACE('',(#923),#644,.T.);
#5125=ADVANCED_FACE('',(#924),#268,.T.);
#5126=ADVANCED_FACE('',(#925),#645,.T.);
#5127=ADVANCED_FACE('',(#926),#646,.T.);
#5128=ADVANCED_FACE('',(#927),#647,.T.);
#5129=ADVANCED_FACE('',(#928),#648,.T.);
#5130=ADVANCED_FACE('',(#929),#649,.T.);
#5131=ADVANCED_FACE('',(#930),#650,.T.);
#5132=ADVANCED_FACE('',(#931),#651,.T.);
#5133=ADVANCED_FACE('',(#932,#476),#652,.F.);
#5134=ADVANCED_FACE('',(#933),#269,.T.);
#5135=ADVANCED_FACE('',(#934),#270,.T.);
#5136=ADVANCED_FACE('',(#935),#653,.T.);
#5137=ADVANCED_FACE('',(#936),#654,.T.);
#5138=ADVANCED_FACE('',(#937),#655,.T.);
#5139=ADVANCED_FACE('',(#938),#4864,.F.);
#5140=ADVANCED_FACE('',(#939),#656,.T.);
#5141=ADVANCED_FACE('',(#940),#657,.T.);
#5142=ADVANCED_FACE('',(#941),#658,.T.);
#5143=ADVANCED_FACE('',(#942,#477),#659,.T.);
#5144=ADVANCED_FACE('',(#943,#478),#660,.F.);
#5145=ADVANCED_FACE('',(#944),#4865,.T.);
#5146=ADVANCED_FACE('',(#945),#661,.T.);
#5147=ADVANCED_FACE('',(#946),#662,.F.);
#5148=ADVANCED_FACE('',(#947),#4866,.F.);
#5149=ADVANCED_FACE('',(#948),#663,.T.);
#5150=ADVANCED_FACE('',(#949),#271,.T.);
#5151=ADVANCED_FACE('',(#950),#4867,.T.);
#5152=ADVANCED_FACE('',(#951,#479),#664,.T.);
#5153=ADVANCED_FACE('',(#952,#480),#4868,.T.);
#5154=ADVANCED_FACE('',(#953),#272,.T.);
#5155=ADVANCED_FACE('',(#954),#665,.T.);
#5156=ADVANCED_FACE('',(#955),#4869,.F.);
#5157=ADVANCED_FACE('',(#956),#4870,.T.);
#5158=ADVANCED_FACE('',(#957,#481),#666,.T.);
#5159=ADVANCED_FACE('',(#958,#482),#667,.F.);
#5160=ADVANCED_FACE('',(#959),#4871,.F.);
#5161=ADVANCED_FACE('',(#960),#4872,.T.);
#5162=ADVANCED_FACE('',(#961,#483),#668,.T.);
#5163=ADVANCED_FACE('',(#962,#484),#669,.F.);
#5164=ADVANCED_FACE('',(#963,#485),#11,.T.);
#5165=ADVANCED_FACE('',(#964),#670,.F.);
#5166=ADVANCED_FACE('',(#965),#671,.T.);
#5167=ADVANCED_FACE('',(#966),#4873,.T.);
#5168=ADVANCED_FACE('',(#967),#672,.F.);
#5169=CLOSED_SHELL('',(#4874,#4875,#4876,#4877,#4878,#4879,#4880,#4881,
#4882,#4883,#4884,#4885,#4886,#4887,#4888,#4889,#4890,#4891,#4892,#4893,
#4894,#4895,#4896,#4897,#4898,#4899,#4900,#4901,#4902,#4903,#4904,#4905,
#4906));
#5170=CLOSED_SHELL('',(#4907,#4908,#4909,#4910,#4911,#4912,#4913,#4914,
#4915,#4916,#4917,#4918,#4919,#4920,#4921,#4922,#4923,#4924,#4925,#4926,
#4927,#4928,#4929,#4930));
#5171=CLOSED_SHELL('',(#4931,#4932,#4933,#4934,#4935));
#5172=CLOSED_SHELL('',(#4936,#4937,#4938,#4939,#4940,#4941,#4942,#4943));
#5173=CLOSED_SHELL('',(#4944,#4945,#4946,#4947,#4948,#4949,#4950,#4951));
#5174=CLOSED_SHELL('',(#4952,#4953,#4954,#4955,#4956,#4957,#4958,#4959,
#4960,#4961,#4962,#4963,#4964,#4965,#4966,#4967,#4968,#4969,#4970,#4971,
#4972,#4973,#4974,#4975,#4976,#4977,#4978,#4979,#4980,#4981,#4982,#4983,
#4984,#4985));
#5175=CLOSED_SHELL('',(#4986,#4987,#4988,#4989,#4990,#4991,#4992,#4993));
#5176=CLOSED_SHELL('',(#4994,#4995,#4996,#4997,#4998,#4999,#5000,#5001,
#5002,#5003,#5004,#5005));
#5177=CLOSED_SHELL('',(#5006,#5007,#5008,#5009,#5010,#5011,#5012,#5013,
#5014,#5015,#5016));
#5178=CLOSED_SHELL('',(#5017,#5018,#5019,#5020,#5021));
#5179=CLOSED_SHELL('',(#5022,#5023,#5024,#5025));
#5180=CLOSED_SHELL('',(#5026,#5027,#5028,#5029,#5030,#5031,#5032,#5033,
#5034));
#5181=CLOSED_SHELL('',(#5035,#5036,#5037,#5038,#5039,#5040,#5041,#5042));
#5182=CLOSED_SHELL('',(#5043,#5044,#5045,#5046,#5047,#5048,#5049,#5050));
#5183=CLOSED_SHELL('',(#5051,#5052,#5053,#5054,#5055,#5056,#5057,#5058,
#5059,#5060,#5061,#5062,#5063,#5064,#5065,#5066,#5067,#5068,#5069,#5070,
#5071,#5072,#5073,#5074,#5075,#5076));
#5184=CLOSED_SHELL('',(#5077,#5078,#5079,#5080,#5081));
#5185=CLOSED_SHELL('',(#5082,#5083,#5084,#5085,#5086,#5087,#5088,#5089));
#5186=CLOSED_SHELL('',(#5090,#5091,#5092,#5093,#5094,#5095,#5096,#5097));
#5187=CLOSED_SHELL('',(#5098,#5099,#5100,#5101,#5102,#5103,#5104,#5105));
#5188=CLOSED_SHELL('',(#5106,#5107,#5108,#5109,#5110,#5111,#5112,#5113,
#5114,#5115,#5116,#5117,#5118,#5119,#5120,#5121));
#5189=CLOSED_SHELL('',(#5122,#5123,#5124,#5125,#5126,#5127,#5128,#5129,
#5130,#5131,#5132,#5133));
#5190=CLOSED_SHELL('',(#5134,#5135,#5136,#5137,#5138,#5139,#5140,#5141,
#5142,#5143,#5144));
#5191=CLOSED_SHELL('',(#5145,#5146,#5147));
#5192=CLOSED_SHELL('',(#5148,#5149,#5150,#5151,#5152,#5153,#5154,#5155));
#5193=CLOSED_SHELL('',(#5156,#5157,#5158,#5159));
#5194=CLOSED_SHELL('',(#5160,#5161,#5162,#5163));
#5195=CLOSED_SHELL('',(#5164,#5165,#5166,#5167,#5168));
#5196=DERIVED_UNIT_ELEMENT(#5244,1.);
#5197=DERIVED_UNIT_ELEMENT(#9287,-3.);
#5198=DERIVED_UNIT_ELEMENT(#5244,1.);
#5199=DERIVED_UNIT_ELEMENT(#9287,-3.);
#5200=DERIVED_UNIT_ELEMENT(#5244,1.);
#5201=DERIVED_UNIT_ELEMENT(#9287,-3.);
#5202=DERIVED_UNIT_ELEMENT(#5244,1.);
#5203=DERIVED_UNIT_ELEMENT(#9287,-3.);
#5204=DERIVED_UNIT_ELEMENT(#5244,1.);
#5205=DERIVED_UNIT_ELEMENT(#9287,-3.);
#5206=DERIVED_UNIT_ELEMENT(#5244,1.);
#5207=DERIVED_UNIT_ELEMENT(#9287,-3.);
#5208=DERIVED_UNIT_ELEMENT(#5244,1.);
#5209=DERIVED_UNIT_ELEMENT(#9287,-3.);
#5210=DERIVED_UNIT_ELEMENT(#5244,1.);
#5211=DERIVED_UNIT_ELEMENT(#9287,-3.);
#5212=DERIVED_UNIT_ELEMENT(#5244,1.);
#5213=DERIVED_UNIT_ELEMENT(#9287,-3.);
#5214=DERIVED_UNIT_ELEMENT(#5244,1.);
#5215=DERIVED_UNIT_ELEMENT(#9287,-3.);
#5216=DERIVED_UNIT_ELEMENT(#5244,1.);
#5217=DERIVED_UNIT_ELEMENT(#9287,-3.);
#5218=DERIVED_UNIT_ELEMENT(#5244,1.);
#5219=DERIVED_UNIT_ELEMENT(#9287,-3.);
#5220=DERIVED_UNIT_ELEMENT(#5244,1.);
#5221=DERIVED_UNIT_ELEMENT(#9287,-3.);
#5222=DERIVED_UNIT_ELEMENT(#5244,1.);
#5223=DERIVED_UNIT_ELEMENT(#9287,-3.);
#5224=DERIVED_UNIT_ELEMENT(#5244,1.);
#5225=DERIVED_UNIT_ELEMENT(#9287,-3.);
#5226=DERIVED_UNIT_ELEMENT(#5244,1.);
#5227=DERIVED_UNIT_ELEMENT(#9287,-3.);
#5228=DERIVED_UNIT_ELEMENT(#5244,1.);
#5229=DERIVED_UNIT_ELEMENT(#9287,-3.);
#5230=DERIVED_UNIT_ELEMENT(#5244,1.);
#5231=DERIVED_UNIT_ELEMENT(#9287,-3.);
#5232=DERIVED_UNIT_ELEMENT(#5244,1.);
#5233=DERIVED_UNIT_ELEMENT(#9287,-3.);
#5234=DERIVED_UNIT_ELEMENT(#5244,1.);
#5235=DERIVED_UNIT_ELEMENT(#9287,-3.);
#5236=DERIVED_UNIT_ELEMENT(#5244,1.);
#5237=DERIVED_UNIT_ELEMENT(#9287,-3.);
#5238=DERIVED_UNIT_ELEMENT(#5244,1.);
#5239=DERIVED_UNIT_ELEMENT(#9287,-3.);
#5240=DERIVED_UNIT_ELEMENT(#5244,1.);
#5241=DERIVED_UNIT_ELEMENT(#9287,-3.);
#5242=DERIVED_UNIT_ELEMENT(#5244,1.);
#5243=DERIVED_UNIT_ELEMENT(#9287,-3.);
#5244=(
MASS_UNIT()
NAMED_UNIT(*)
SI_UNIT(.KILO.,.GRAM.)
);
#5245=DERIVED_UNIT((#5196,#5197));
#5246=DERIVED_UNIT((#5198,#5199));
#5247=DERIVED_UNIT((#5200,#5201));
#5248=DERIVED_UNIT((#5202,#5203));
#5249=DERIVED_UNIT((#5204,#5205));
#5250=DERIVED_UNIT((#5206,#5207));
#5251=DERIVED_UNIT((#5208,#5209));
#5252=DERIVED_UNIT((#5210,#5211));
#5253=DERIVED_UNIT((#5212,#5213));
#5254=DERIVED_UNIT((#5214,#5215));
#5255=DERIVED_UNIT((#5216,#5217));
#5256=DERIVED_UNIT((#5218,#5219));
#5257=DERIVED_UNIT((#5220,#5221));
#5258=DERIVED_UNIT((#5222,#5223));
#5259=DERIVED_UNIT((#5224,#5225));
#5260=DERIVED_UNIT((#5226,#5227));
#5261=DERIVED_UNIT((#5228,#5229));
#5262=DERIVED_UNIT((#5230,#5231));
#5263=DERIVED_UNIT((#5232,#5233));
#5264=DERIVED_UNIT((#5234,#5235));
#5265=DERIVED_UNIT((#5236,#5237));
#5266=DERIVED_UNIT((#5238,#5239));
#5267=DERIVED_UNIT((#5240,#5241));
#5268=DERIVED_UNIT((#5242,#5243));
#5269=MEASURE_REPRESENTATION_ITEM('density measure',
POSITIVE_RATIO_MEASURE(7850.),#5245);
#5270=MEASURE_REPRESENTATION_ITEM('density measure',
POSITIVE_RATIO_MEASURE(7850.),#5246);
#5271=MEASURE_REPRESENTATION_ITEM('density measure',
POSITIVE_RATIO_MEASURE(7850.),#5247);
#5272=MEASURE_REPRESENTATION_ITEM('density measure',
POSITIVE_RATIO_MEASURE(7850.),#5248);
#5273=MEASURE_REPRESENTATION_ITEM('density measure',
POSITIVE_RATIO_MEASURE(7850.),#5249);
#5274=MEASURE_REPRESENTATION_ITEM('density measure',
POSITIVE_RATIO_MEASURE(7850.),#5250);
#5275=MEASURE_REPRESENTATION_ITEM('density measure',
POSITIVE_RATIO_MEASURE(7850.),#5251);
#5276=MEASURE_REPRESENTATION_ITEM('density measure',
POSITIVE_RATIO_MEASURE(7850.),#5252);
#5277=MEASURE_REPRESENTATION_ITEM('density measure',
POSITIVE_RATIO_MEASURE(7850.),#5253);
#5278=MEASURE_REPRESENTATION_ITEM('density measure',
POSITIVE_RATIO_MEASURE(7850.),#5254);
#5279=MEASURE_REPRESENTATION_ITEM('density measure',
POSITIVE_RATIO_MEASURE(7850.),#5255);
#5280=MEASURE_REPRESENTATION_ITEM('density measure',
POSITIVE_RATIO_MEASURE(7850.),#5256);
#5281=MEASURE_REPRESENTATION_ITEM('density measure',
POSITIVE_RATIO_MEASURE(7850.),#5257);
#5282=MEASURE_REPRESENTATION_ITEM('density measure',
POSITIVE_RATIO_MEASURE(7850.),#5258);
#5283=MEASURE_REPRESENTATION_ITEM('density measure',
POSITIVE_RATIO_MEASURE(7850.),#5259);
#5284=MEASURE_REPRESENTATION_ITEM('density measure',
POSITIVE_RATIO_MEASURE(7850.),#5260);
#5285=MEASURE_REPRESENTATION_ITEM('density measure',
POSITIVE_RATIO_MEASURE(7850.),#5261);
#5286=MEASURE_REPRESENTATION_ITEM('density measure',
POSITIVE_RATIO_MEASURE(7850.),#5262);
#5287=MEASURE_REPRESENTATION_ITEM('density measure',
POSITIVE_RATIO_MEASURE(7850.),#5263);
#5288=MEASURE_REPRESENTATION_ITEM('density measure',
POSITIVE_RATIO_MEASURE(7850.),#5264);
#5289=MEASURE_REPRESENTATION_ITEM('density measure',
POSITIVE_RATIO_MEASURE(7850.),#5265);
#5290=MEASURE_REPRESENTATION_ITEM('density measure',
POSITIVE_RATIO_MEASURE(7850.),#5266);
#5291=MEASURE_REPRESENTATION_ITEM('density measure',
POSITIVE_RATIO_MEASURE(7850.),#5267);
#5292=MEASURE_REPRESENTATION_ITEM('density measure',
POSITIVE_RATIO_MEASURE(7850.),#5268);
#5293=PROPERTY_DEFINITION_REPRESENTATION(#5413,#5341);
#5294=PROPERTY_DEFINITION_REPRESENTATION(#5414,#5342);
#5295=PROPERTY_DEFINITION_REPRESENTATION(#5415,#5343);
#5296=PROPERTY_DEFINITION_REPRESENTATION(#5416,#5344);
#5297=PROPERTY_DEFINITION_REPRESENTATION(#5417,#5345);
#5298=PROPERTY_DEFINITION_REPRESENTATION(#5418,#5346);
#5299=PROPERTY_DEFINITION_REPRESENTATION(#5419,#5347);
#5300=PROPERTY_DEFINITION_REPRESENTATION(#5420,#5348);
#5301=PROPERTY_DEFINITION_REPRESENTATION(#5421,#5349);
#5302=PROPERTY_DEFINITION_REPRESENTATION(#5422,#5350);
#5303=PROPERTY_DEFINITION_REPRESENTATION(#5423,#5351);
#5304=PROPERTY_DEFINITION_REPRESENTATION(#5424,#5352);
#5305=PROPERTY_DEFINITION_REPRESENTATION(#5425,#5353);
#5306=PROPERTY_DEFINITION_REPRESENTATION(#5426,#5354);
#5307=PROPERTY_DEFINITION_REPRESENTATION(#5427,#5355);
#5308=PROPERTY_DEFINITION_REPRESENTATION(#5428,#5356);
#5309=PROPERTY_DEFINITION_REPRESENTATION(#5429,#5357);
#5310=PROPERTY_DEFINITION_REPRESENTATION(#5430,#5358);
#5311=PROPERTY_DEFINITION_REPRESENTATION(#5431,#5359);
#5312=PROPERTY_DEFINITION_REPRESENTATION(#5432,#5360);
#5313=PROPERTY_DEFINITION_REPRESENTATION(#5433,#5361);
#5314=PROPERTY_DEFINITION_REPRESENTATION(#5434,#5362);
#5315=PROPERTY_DEFINITION_REPRESENTATION(#5435,#5363);
#5316=PROPERTY_DEFINITION_REPRESENTATION(#5436,#5364);
#5317=PROPERTY_DEFINITION_REPRESENTATION(#5437,#5365);
#5318=PROPERTY_DEFINITION_REPRESENTATION(#5438,#5366);
#5319=PROPERTY_DEFINITION_REPRESENTATION(#5439,#5367);
#5320=PROPERTY_DEFINITION_REPRESENTATION(#5440,#5368);
#5321=PROPERTY_DEFINITION_REPRESENTATION(#5441,#5369);
#5322=PROPERTY_DEFINITION_REPRESENTATION(#5442,#5370);
#5323=PROPERTY_DEFINITION_REPRESENTATION(#5443,#5371);
#5324=PROPERTY_DEFINITION_REPRESENTATION(#5444,#5372);
#5325=PROPERTY_DEFINITION_REPRESENTATION(#5445,#5373);
#5326=PROPERTY_DEFINITION_REPRESENTATION(#5446,#5374);
#5327=PROPERTY_DEFINITION_REPRESENTATION(#5447,#5375);
#5328=PROPERTY_DEFINITION_REPRESENTATION(#5448,#5376);
#5329=PROPERTY_DEFINITION_REPRESENTATION(#5449,#5377);
#5330=PROPERTY_DEFINITION_REPRESENTATION(#5450,#5378);
#5331=PROPERTY_DEFINITION_REPRESENTATION(#5451,#5379);
#5332=PROPERTY_DEFINITION_REPRESENTATION(#5452,#5380);
#5333=PROPERTY_DEFINITION_REPRESENTATION(#5453,#5381);
#5334=PROPERTY_DEFINITION_REPRESENTATION(#5454,#5382);
#5335=PROPERTY_DEFINITION_REPRESENTATION(#5455,#5383);
#5336=PROPERTY_DEFINITION_REPRESENTATION(#5456,#5384);
#5337=PROPERTY_DEFINITION_REPRESENTATION(#5457,#5385);
#5338=PROPERTY_DEFINITION_REPRESENTATION(#5458,#5386);
#5339=PROPERTY_DEFINITION_REPRESENTATION(#5459,#5387);
#5340=PROPERTY_DEFINITION_REPRESENTATION(#5460,#5388);
#5341=REPRESENTATION('material name',(#5389),#9258);
#5342=REPRESENTATION('density',(#5269),#9258);
#5343=REPRESENTATION('material name',(#5390),#9259);
#5344=REPRESENTATION('density',(#5270),#9259);
#5345=REPRESENTATION('material name',(#5391),#9260);
#5346=REPRESENTATION('density',(#5271),#9260);
#5347=REPRESENTATION('material name',(#5392),#9261);
#5348=REPRESENTATION('density',(#5272),#9261);
#5349=REPRESENTATION('material name',(#5393),#9262);
#5350=REPRESENTATION('density',(#5273),#9262);
#5351=REPRESENTATION('material name',(#5394),#9263);
#5352=REPRESENTATION('density',(#5274),#9263);
#5353=REPRESENTATION('material name',(#5395),#9264);
#5354=REPRESENTATION('density',(#5275),#9264);
#5355=REPRESENTATION('material name',(#5396),#9265);
#5356=REPRESENTATION('density',(#5276),#9265);
#5357=REPRESENTATION('material name',(#5397),#9266);
#5358=REPRESENTATION('density',(#5277),#9266);
#5359=REPRESENTATION('material name',(#5398),#9267);
#5360=REPRESENTATION('density',(#5278),#9267);
#5361=REPRESENTATION('material name',(#5399),#9268);
#5362=REPRESENTATION('density',(#5279),#9268);
#5363=REPRESENTATION('material name',(#5400),#9269);
#5364=REPRESENTATION('density',(#5280),#9269);
#5365=REPRESENTATION('material name',(#5401),#9271);
#5366=REPRESENTATION('density',(#5281),#9271);
#5367=REPRESENTATION('material name',(#5402),#9272);
#5368=REPRESENTATION('density',(#5282),#9272);
#5369=REPRESENTATION('material name',(#5403),#9273);
#5370=REPRESENTATION('density',(#5283),#9273);
#5371=REPRESENTATION('material name',(#5404),#9275);
#5372=REPRESENTATION('density',(#5284),#9275);
#5373=REPRESENTATION('material name',(#5405),#9277);
#5374=REPRESENTATION('density',(#5285),#9277);
#5375=REPRESENTATION('material name',(#5406),#9278);
#5376=REPRESENTATION('density',(#5286),#9278);
#5377=REPRESENTATION('material name',(#5407),#9279);
#5378=REPRESENTATION('density',(#5287),#9279);
#5379=REPRESENTATION('material name',(#5408),#9280);
#5380=REPRESENTATION('density',(#5288),#9280);
#5381=REPRESENTATION('material name',(#5409),#9281);
#5382=REPRESENTATION('density',(#5289),#9281);
#5383=REPRESENTATION('material name',(#5410),#9282);
#5384=REPRESENTATION('density',(#5290),#9282);
#5385=REPRESENTATION('material name',(#5411),#9283);
#5386=REPRESENTATION('density',(#5291),#9283);
#5387=REPRESENTATION('material name',(#5412),#9284);
#5388=REPRESENTATION('density',(#5292),#9284);
#5389=DESCRIPTIVE_REPRESENTATION_ITEM('Steel','Steel');
#5390=DESCRIPTIVE_REPRESENTATION_ITEM('Steel','Steel');
#5391=DESCRIPTIVE_REPRESENTATION_ITEM('Steel','Steel');
#5392=DESCRIPTIVE_REPRESENTATION_ITEM('Steel','Steel');
#5393=DESCRIPTIVE_REPRESENTATION_ITEM('Steel','Steel');
#5394=DESCRIPTIVE_REPRESENTATION_ITEM('Steel','Steel');
#5395=DESCRIPTIVE_REPRESENTATION_ITEM('Steel','Steel');
#5396=DESCRIPTIVE_REPRESENTATION_ITEM('Steel','Steel');
#5397=DESCRIPTIVE_REPRESENTATION_ITEM('Steel','Steel');
#5398=DESCRIPTIVE_REPRESENTATION_ITEM('Steel','Steel');
#5399=DESCRIPTIVE_REPRESENTATION_ITEM('Steel','Steel');
#5400=DESCRIPTIVE_REPRESENTATION_ITEM('Steel','Steel');
#5401=DESCRIPTIVE_REPRESENTATION_ITEM('Steel','Steel');
#5402=DESCRIPTIVE_REPRESENTATION_ITEM('Steel','Steel');
#5403=DESCRIPTIVE_REPRESENTATION_ITEM('Steel','Steel');
#5404=DESCRIPTIVE_REPRESENTATION_ITEM('Steel','Steel');
#5405=DESCRIPTIVE_REPRESENTATION_ITEM('Steel','Steel');
#5406=DESCRIPTIVE_REPRESENTATION_ITEM('Steel','Steel');
#5407=DESCRIPTIVE_REPRESENTATION_ITEM('Steel','Steel');
#5408=DESCRIPTIVE_REPRESENTATION_ITEM('Steel','Steel');
#5409=DESCRIPTIVE_REPRESENTATION_ITEM('Steel','Steel');
#5410=DESCRIPTIVE_REPRESENTATION_ITEM('Steel','Steel');
#5411=DESCRIPTIVE_REPRESENTATION_ITEM('Steel','Steel');
#5412=DESCRIPTIVE_REPRESENTATION_ITEM('Steel','Steel');
#5413=PROPERTY_DEFINITION('material property','material name',#9426);
#5414=PROPERTY_DEFINITION('material property','density of part',#9426);
#5415=PROPERTY_DEFINITION('material property','material name',#9427);
#5416=PROPERTY_DEFINITION('material property','density of part',#9427);
#5417=PROPERTY_DEFINITION('material property','material name',#9428);
#5418=PROPERTY_DEFINITION('material property','density of part',#9428);
#5419=PROPERTY_DEFINITION('material property','material name',#9429);
#5420=PROPERTY_DEFINITION('material property','density of part',#9429);
#5421=PROPERTY_DEFINITION('material property','material name',#9430);
#5422=PROPERTY_DEFINITION('material property','density of part',#9430);
#5423=PROPERTY_DEFINITION('material property','material name',#9431);
#5424=PROPERTY_DEFINITION('material property','density of part',#9431);
#5425=PROPERTY_DEFINITION('material property','material name',#9432);
#5426=PROPERTY_DEFINITION('material property','density of part',#9432);
#5427=PROPERTY_DEFINITION('material property','material name',#9433);
#5428=PROPERTY_DEFINITION('material property','density of part',#9433);
#5429=PROPERTY_DEFINITION('material property','material name',#9434);
#5430=PROPERTY_DEFINITION('material property','density of part',#9434);
#5431=PROPERTY_DEFINITION('material property','material name',#9435);
#5432=PROPERTY_DEFINITION('material property','density of part',#9435);
#5433=PROPERTY_DEFINITION('material property','material name',#9436);
#5434=PROPERTY_DEFINITION('material property','density of part',#9436);
#5435=PROPERTY_DEFINITION('material property','material name',#9437);
#5436=PROPERTY_DEFINITION('material property','density of part',#9437);
#5437=PROPERTY_DEFINITION('material property','material name',#9439);
#5438=PROPERTY_DEFINITION('material property','density of part',#9439);
#5439=PROPERTY_DEFINITION('material property','material name',#9440);
#5440=PROPERTY_DEFINITION('material property','density of part',#9440);
#5441=PROPERTY_DEFINITION('material property','material name',#9441);
#5442=PROPERTY_DEFINITION('material property','density of part',#9441);
#5443=PROPERTY_DEFINITION('material property','material name',#9443);
#5444=PROPERTY_DEFINITION('material property','density of part',#9443);
#5445=PROPERTY_DEFINITION('material property','material name',#9445);
#5446=PROPERTY_DEFINITION('material property','density of part',#9445);
#5447=PROPERTY_DEFINITION('material property','material name',#9446);
#5448=PROPERTY_DEFINITION('material property','density of part',#9446);
#5449=PROPERTY_DEFINITION('material property','material name',#9447);
#5450=PROPERTY_DEFINITION('material property','density of part',#9447);
#5451=PROPERTY_DEFINITION('material property','material name',#9448);
#5452=PROPERTY_DEFINITION('material property','density of part',#9448);
#5453=PROPERTY_DEFINITION('material property','material name',#9449);
#5454=PROPERTY_DEFINITION('material property','density of part',#9449);
#5455=PROPERTY_DEFINITION('material property','material name',#9450);
#5456=PROPERTY_DEFINITION('material property','density of part',#9450);
#5457=PROPERTY_DEFINITION('material property','material name',#9451);
#5458=PROPERTY_DEFINITION('material property','density of part',#9451);
#5459=PROPERTY_DEFINITION('material property','material name',#9452);
#5460=PROPERTY_DEFINITION('material property','density of part',#9452);
#5461=AXIS2_PLACEMENT_3D('',#7575,#6029,#6030);
#5462=AXIS2_PLACEMENT_3D('',#7576,#6031,#6032);
#5463=AXIS2_PLACEMENT_3D('',#7577,#6033,#6034);
#5464=AXIS2_PLACEMENT_3D('',#7578,#6035,#6036);
#5465=AXIS2_PLACEMENT_3D('',#7583,#6038,#6039);
#5466=AXIS2_PLACEMENT_3D('',#7587,#6041,#6042);
#5467=AXIS2_PLACEMENT_3D('',#7590,#6044,#6045);
#5468=AXIS2_PLACEMENT_3D('',#7591,#6046,#6047);
#5469=AXIS2_PLACEMENT_3D('',#7592,#6048,#6049);
#5470=AXIS2_PLACEMENT_3D('',#7593,#6050,#6051);
#5471=AXIS2_PLACEMENT_3D('',#7611,#6061,#6062);
#5472=AXIS2_PLACEMENT_3D('',#7615,#6065,#6066);
#5473=AXIS2_PLACEMENT_3D('',#7619,#6069,#6070);
#5474=AXIS2_PLACEMENT_3D('',#7623,#6073,#6074);
#5475=AXIS2_PLACEMENT_3D('',#7627,#6077,#6078);
#5476=AXIS2_PLACEMENT_3D('',#7629,#6080,#6081);
#5477=AXIS2_PLACEMENT_3D('',#7660,#6097,#6098);
#5478=AXIS2_PLACEMENT_3D('',#7662,#6099,#6100);
#5479=AXIS2_PLACEMENT_3D('',#7663,#6101,#6102);
#5480=AXIS2_PLACEMENT_3D('',#7665,#6103,#6104);
#5481=AXIS2_PLACEMENT_3D('',#7667,#6106,#6107);
#5482=AXIS2_PLACEMENT_3D('',#7669,#6108,#6109);
#5483=AXIS2_PLACEMENT_3D('',#7671,#6111,#6112);
#5484=AXIS2_PLACEMENT_3D('',#7673,#6113,#6114);
#5485=AXIS2_PLACEMENT_3D('',#7676,#6116,#6117);
#5486=AXIS2_PLACEMENT_3D('',#7677,#6118,#6119);
#5487=AXIS2_PLACEMENT_3D('',#7683,#6123,#6124);
#5488=AXIS2_PLACEMENT_3D('',#7687,#6127,#6128);
#5489=AXIS2_PLACEMENT_3D('',#7691,#6131,#6132);
#5490=AXIS2_PLACEMENT_3D('',#7693,#6134,#6135);
#5491=AXIS2_PLACEMENT_3D('',#7694,#6136,#6137);
#5492=AXIS2_PLACEMENT_3D('',#7696,#6138,#6139);
#5493=AXIS2_PLACEMENT_3D('',#7699,#6141,#6142);
#5494=AXIS2_PLACEMENT_3D('',#7700,#6143,#6144);
#5495=AXIS2_PLACEMENT_3D('',#7702,#6145,#6146);
#5496=AXIS2_PLACEMENT_3D('',#7705,#6148,#6149);
#5497=AXIS2_PLACEMENT_3D('',#7706,#6150,#6151);
#5498=AXIS2_PLACEMENT_3D('',#7712,#6155,#6156);
#5499=AXIS2_PLACEMENT_3D('',#7716,#6159,#6160);
#5500=AXIS2_PLACEMENT_3D('',#7720,#6163,#6164);
#5501=AXIS2_PLACEMENT_3D('',#7722,#6166,#6167);
#5502=AXIS2_PLACEMENT_3D('',#7723,#6168,#6169);
#5503=AXIS2_PLACEMENT_3D('',#7729,#6173,#6174);
#5504=AXIS2_PLACEMENT_3D('',#7733,#6177,#6178);
#5505=AXIS2_PLACEMENT_3D('',#7737,#6181,#6182);
#5506=AXIS2_PLACEMENT_3D('',#7739,#6184,#6185);
#5507=AXIS2_PLACEMENT_3D('',#7740,#6186,#6187);
#5508=AXIS2_PLACEMENT_3D('',#7744,#6190,#6191);
#5509=AXIS2_PLACEMENT_3D('',#7748,#6194,#6195);
#5510=AXIS2_PLACEMENT_3D('',#7750,#6197,#6198);
#5511=AXIS2_PLACEMENT_3D('',#7751,#6199,#6200);
#5512=AXIS2_PLACEMENT_3D('',#7752,#6201,#6202);
#5513=AXIS2_PLACEMENT_3D('',#7757,#6204,#6205);
#5514=AXIS2_PLACEMENT_3D('',#7760,#6207,#6208);
#5515=AXIS2_PLACEMENT_3D('',#7761,#6209,#6210);
#5516=AXIS2_PLACEMENT_3D('',#7763,#6212,#6213);
#5517=AXIS2_PLACEMENT_3D('',#7774,#6219,#6220);
#5518=AXIS2_PLACEMENT_3D('',#7776,#6221,#6222);
#5519=AXIS2_PLACEMENT_3D('',#7777,#6223,#6224);
#5520=AXIS2_PLACEMENT_3D('',#7780,#6226,#6227);
#5521=AXIS2_PLACEMENT_3D('',#7781,#6228,#6229);
#5522=AXIS2_PLACEMENT_3D('',#7784,#6231,#6232);
#5523=AXIS2_PLACEMENT_3D('',#7785,#6233,#6234);
#5524=AXIS2_PLACEMENT_3D('',#7791,#6238,#6239);
#5525=AXIS2_PLACEMENT_3D('',#7793,#6240,#6241);
#5526=AXIS2_PLACEMENT_3D('',#7796,#6243,#6244);
#5527=AXIS2_PLACEMENT_3D('',#7797,#6245,#6246);
#5528=AXIS2_PLACEMENT_3D('',#7798,#6247,#6248);
#5529=AXIS2_PLACEMENT_3D('',#7804,#6252,#6253);
#5530=AXIS2_PLACEMENT_3D('',#7813,#6258,#6259);
#5531=AXIS2_PLACEMENT_3D('',#7816,#6262,#6263);
#5532=AXIS2_PLACEMENT_3D('',#7822,#6267,#6268);
#5533=AXIS2_PLACEMENT_3D('',#7824,#6269,#6270);
#5534=AXIS2_PLACEMENT_3D('',#7827,#6272,#6273);
#5535=AXIS2_PLACEMENT_3D('',#7828,#6274,#6275);
#5536=AXIS2_PLACEMENT_3D('',#7829,#6276,#6277);
#5537=AXIS2_PLACEMENT_3D('',#7835,#6281,#6282);
#5538=AXIS2_PLACEMENT_3D('',#7844,#6287,#6288);
#5539=AXIS2_PLACEMENT_3D('',#7847,#6291,#6292);
#5540=AXIS2_PLACEMENT_3D('',#7853,#6296,#6297);
#5541=AXIS2_PLACEMENT_3D('',#7859,#6301,#6302);
#5542=AXIS2_PLACEMENT_3D('',#7865,#6306,#6307);
#5543=AXIS2_PLACEMENT_3D('',#7869,#6310,#6311);
#5544=AXIS2_PLACEMENT_3D('',#7873,#6314,#6315);
#5545=AXIS2_PLACEMENT_3D('',#7875,#6317,#6318);
#5546=AXIS2_PLACEMENT_3D('',#7876,#6319,#6320);
#5547=AXIS2_PLACEMENT_3D('',#7877,#6321,#6322);
#5548=AXIS2_PLACEMENT_3D('',#7879,#6323,#6324);
#5549=AXIS2_PLACEMENT_3D('',#7882,#6326,#6327);
#5550=AXIS2_PLACEMENT_3D('',#7883,#6328,#6329);
#5551=AXIS2_PLACEMENT_3D('',#7886,#6331,#6332);
#5552=AXIS2_PLACEMENT_3D('',#7887,#6333,#6334);
#5553=AXIS2_PLACEMENT_3D('',#7889,#6335,#6336);
#5554=AXIS2_PLACEMENT_3D('',#7890,#6337,#6338);
#5555=AXIS2_PLACEMENT_3D('',#7893,#6340,#6341);
#5556=AXIS2_PLACEMENT_3D('',#7894,#6342,#6343);
#5557=AXIS2_PLACEMENT_3D('',#7895,#6344,#6345);
#5558=AXIS2_PLACEMENT_3D('',#7896,#6346,#6347);
#5559=AXIS2_PLACEMENT_3D('',#7905,#6352,#6353);
#5560=AXIS2_PLACEMENT_3D('',#7911,#6357,#6358);
#5561=AXIS2_PLACEMENT_3D('',#7917,#6362,#6363);
#5562=AXIS2_PLACEMENT_3D('',#7923,#6367,#6368);
#5563=AXIS2_PLACEMENT_3D('',#7929,#6372,#6373);
#5564=AXIS2_PLACEMENT_3D('',#7932,#6376,#6377);
#5565=AXIS2_PLACEMENT_3D('',#7933,#6378,#6379);
#5566=AXIS2_PLACEMENT_3D('',#7934,#6380,#6381);
#5567=AXIS2_PLACEMENT_3D('',#7936,#6382,#6383);
#5568=AXIS2_PLACEMENT_3D('',#7937,#6384,#6385);
#5569=AXIS2_PLACEMENT_3D('',#7939,#6386,#6387);
#5570=AXIS2_PLACEMENT_3D('',#7940,#6388,#6389);
#5571=AXIS2_PLACEMENT_3D('',#7942,#6390,#6391);
#5572=AXIS2_PLACEMENT_3D('',#7944,#6393,#6394);
#5573=AXIS2_PLACEMENT_3D('',#7946,#6395,#6396);
#5574=AXIS2_PLACEMENT_3D('',#7948,#6398,#6399);
#5575=AXIS2_PLACEMENT_3D('',#7950,#6400,#6401);
#5576=AXIS2_PLACEMENT_3D('',#7952,#6403,#6404);
#5577=AXIS2_PLACEMENT_3D('',#7954,#6405,#6406);
#5578=AXIS2_PLACEMENT_3D('',#7955,#6407,#6408);
#5579=AXIS2_PLACEMENT_3D('',#7957,#6409,#6410);
#5580=AXIS2_PLACEMENT_3D('',#7959,#6412,#6413);
#5581=AXIS2_PLACEMENT_3D('',#7961,#6415,#6416);
#5582=AXIS2_PLACEMENT_3D('',#7962,#6417,#6418);
#5583=AXIS2_PLACEMENT_3D('',#7964,#6419,#6420);
#5584=AXIS2_PLACEMENT_3D('',#7967,#6422,#6423);
#5585=AXIS2_PLACEMENT_3D('',#7968,#6424,#6425);
#5586=AXIS2_PLACEMENT_3D('',#7970,#6426,#6427);
#5587=AXIS2_PLACEMENT_3D('',#7973,#6429,#6430);
#5588=AXIS2_PLACEMENT_3D('',#7974,#6431,#6432);
#5589=AXIS2_PLACEMENT_3D('',#7976,#6433,#6434);
#5590=AXIS2_PLACEMENT_3D('',#7979,#6436,#6437);
#5591=AXIS2_PLACEMENT_3D('',#7980,#6438,#6439);
#5592=AXIS2_PLACEMENT_3D('',#7982,#6440,#6441);
#5593=AXIS2_PLACEMENT_3D('',#7985,#6443,#6444);
#5594=AXIS2_PLACEMENT_3D('',#7986,#6445,#6446);
#5595=AXIS2_PLACEMENT_3D('',#7988,#6447,#6448);
#5596=AXIS2_PLACEMENT_3D('',#7991,#6450,#6451);
#5597=AXIS2_PLACEMENT_3D('',#7992,#6452,#6453);
#5598=AXIS2_PLACEMENT_3D('',#7994,#6454,#6455);
#5599=AXIS2_PLACEMENT_3D('',#7997,#6457,#6458);
#5600=AXIS2_PLACEMENT_3D('',#7998,#6459,#6460);
#5601=AXIS2_PLACEMENT_3D('',#8000,#6461,#6462);
#5602=AXIS2_PLACEMENT_3D('',#8003,#6464,#6465);
#5603=AXIS2_PLACEMENT_3D('',#8004,#6466,#6467);
#5604=AXIS2_PLACEMENT_3D('',#8006,#6468,#6469);
#5605=AXIS2_PLACEMENT_3D('',#8009,#6471,#6472);
#5606=AXIS2_PLACEMENT_3D('',#8010,#6473,#6474);
#5607=AXIS2_PLACEMENT_3D('',#8012,#6475,#6476);
#5608=AXIS2_PLACEMENT_3D('',#8015,#6478,#6479);
#5609=AXIS2_PLACEMENT_3D('',#8016,#6480,#6481);
#5610=AXIS2_PLACEMENT_3D('',#8018,#6482,#6483);
#5611=AXIS2_PLACEMENT_3D('',#8021,#6485,#6486);
#5612=AXIS2_PLACEMENT_3D('',#8022,#6487,#6488);
#5613=AXIS2_PLACEMENT_3D('',#8024,#6489,#6490);
#5614=AXIS2_PLACEMENT_3D('',#8027,#6492,#6493);
#5615=AXIS2_PLACEMENT_3D('',#8028,#6494,#6495);
#5616=AXIS2_PLACEMENT_3D('',#8030,#6496,#6497);
#5617=AXIS2_PLACEMENT_3D('',#8033,#6499,#6500);
#5618=AXIS2_PLACEMENT_3D('',#8034,#6501,#6502);
#5619=AXIS2_PLACEMENT_3D('',#8036,#6503,#6504);
#5620=AXIS2_PLACEMENT_3D('',#8039,#6506,#6507);
#5621=AXIS2_PLACEMENT_3D('',#8040,#6508,#6509);
#5622=AXIS2_PLACEMENT_3D('',#8042,#6510,#6511);
#5623=AXIS2_PLACEMENT_3D('',#8045,#6513,#6514);
#5624=AXIS2_PLACEMENT_3D('',#8046,#6515,#6516);
#5625=AXIS2_PLACEMENT_3D('',#8048,#6517,#6518);
#5626=AXIS2_PLACEMENT_3D('',#8051,#6520,#6521);
#5627=AXIS2_PLACEMENT_3D('',#8052,#6522,#6523);
#5628=AXIS2_PLACEMENT_3D('',#8054,#6524,#6525);
#5629=AXIS2_PLACEMENT_3D('',#8057,#6527,#6528);
#5630=AXIS2_PLACEMENT_3D('',#8058,#6529,#6530);
#5631=AXIS2_PLACEMENT_3D('',#8060,#6531,#6532);
#5632=AXIS2_PLACEMENT_3D('',#8063,#6534,#6535);
#5633=AXIS2_PLACEMENT_3D('',#8064,#6536,#6537);
#5634=AXIS2_PLACEMENT_3D('',#8066,#6538,#6539);
#5635=AXIS2_PLACEMENT_3D('',#8069,#6541,#6542);
#5636=AXIS2_PLACEMENT_3D('',#8070,#6543,#6544);
#5637=AXIS2_PLACEMENT_3D('',#8072,#6545,#6546);
#5638=AXIS2_PLACEMENT_3D('',#8075,#6548,#6549);
#5639=AXIS2_PLACEMENT_3D('',#8076,#6550,#6551);
#5640=AXIS2_PLACEMENT_3D('',#8078,#6552,#6553);
#5641=AXIS2_PLACEMENT_3D('',#8081,#6555,#6556);
#5642=AXIS2_PLACEMENT_3D('',#8082,#6557,#6558);
#5643=AXIS2_PLACEMENT_3D('',#8084,#6559,#6560);
#5644=AXIS2_PLACEMENT_3D('',#8087,#6562,#6563);
#5645=AXIS2_PLACEMENT_3D('',#8088,#6564,#6565);
#5646=AXIS2_PLACEMENT_3D('',#8090,#6566,#6567);
#5647=AXIS2_PLACEMENT_3D('',#8093,#6569,#6570);
#5648=AXIS2_PLACEMENT_3D('',#8094,#6571,#6572);
#5649=AXIS2_PLACEMENT_3D('',#8096,#6573,#6574);
#5650=AXIS2_PLACEMENT_3D('',#8099,#6576,#6577);
#5651=AXIS2_PLACEMENT_3D('',#8100,#6578,#6579);
#5652=AXIS2_PLACEMENT_3D('',#8102,#6580,#6581);
#5653=AXIS2_PLACEMENT_3D('',#8105,#6583,#6584);
#5654=AXIS2_PLACEMENT_3D('',#8106,#6585,#6586);
#5655=AXIS2_PLACEMENT_3D('',#8108,#6587,#6588);
#5656=AXIS2_PLACEMENT_3D('',#8111,#6590,#6591);
#5657=AXIS2_PLACEMENT_3D('',#8112,#6592,#6593);
#5658=AXIS2_PLACEMENT_3D('',#8114,#6594,#6595);
#5659=AXIS2_PLACEMENT_3D('',#8117,#6597,#6598);
#5660=AXIS2_PLACEMENT_3D('',#8118,#6599,#6600);
#5661=AXIS2_PLACEMENT_3D('',#8120,#6601,#6602);
#5662=AXIS2_PLACEMENT_3D('',#8123,#6604,#6605);
#5663=AXIS2_PLACEMENT_3D('',#8124,#6606,#6607);
#5664=AXIS2_PLACEMENT_3D('',#8126,#6608,#6609);
#5665=AXIS2_PLACEMENT_3D('',#8129,#6611,#6612);
#5666=AXIS2_PLACEMENT_3D('',#8130,#6613,#6614);
#5667=AXIS2_PLACEMENT_3D('',#8139,#6619,#6620);
#5668=AXIS2_PLACEMENT_3D('',#8145,#6624,#6625);
#5669=AXIS2_PLACEMENT_3D('',#8151,#6629,#6630);
#5670=AXIS2_PLACEMENT_3D('',#8154,#6633,#6634);
#5671=AXIS2_PLACEMENT_3D('',#8155,#6635,#6636);
#5672=AXIS2_PLACEMENT_3D('',#8156,#6637,#6638);
#5673=AXIS2_PLACEMENT_3D('',#8157,#6639,#6640);
#5674=AXIS2_PLACEMENT_3D('',#8159,#6641,#6642);
#5675=AXIS2_PLACEMENT_3D('',#8162,#6644,#6645);
#5676=AXIS2_PLACEMENT_3D('',#8163,#6646,#6647);
#5677=AXIS2_PLACEMENT_3D('',#8165,#6648,#6649);
#5678=AXIS2_PLACEMENT_3D('',#8168,#6651,#6652);
#5679=AXIS2_PLACEMENT_3D('',#8169,#6653,#6654);
#5680=AXIS2_PLACEMENT_3D('',#8178,#6659,#6660);
#5681=AXIS2_PLACEMENT_3D('',#8184,#6664,#6665);
#5682=AXIS2_PLACEMENT_3D('',#8190,#6669,#6670);
#5683=AXIS2_PLACEMENT_3D('',#8193,#6673,#6674);
#5684=AXIS2_PLACEMENT_3D('',#8194,#6675,#6676);
#5685=AXIS2_PLACEMENT_3D('',#8195,#6677,#6678);
#5686=AXIS2_PLACEMENT_3D('',#8196,#6679,#6680);
#5687=AXIS2_PLACEMENT_3D('',#8198,#6681,#6682);
#5688=AXIS2_PLACEMENT_3D('',#8201,#6684,#6685);
#5689=AXIS2_PLACEMENT_3D('',#8202,#6686,#6687);
#5690=AXIS2_PLACEMENT_3D('',#8204,#6688,#6689);
#5691=AXIS2_PLACEMENT_3D('',#8206,#6691,#6692);
#5692=AXIS2_PLACEMENT_3D('',#8207,#6693,#6694);
#5693=AXIS2_PLACEMENT_3D('',#8209,#6695,#6696);
#5694=AXIS2_PLACEMENT_3D('',#8235,#6698,#6699);
#5695=AXIS2_PLACEMENT_3D('',#8241,#6703,#6704);
#5696=AXIS2_PLACEMENT_3D('',#8245,#6707,#6708);
#5697=AXIS2_PLACEMENT_3D('',#8249,#6711,#6712);
#5698=AXIS2_PLACEMENT_3D('',#8253,#6715,#6716);
#5699=AXIS2_PLACEMENT_3D('',#8257,#6719,#6720);
#5700=AXIS2_PLACEMENT_3D('',#8259,#6722,#6723);
#5701=AXIS2_PLACEMENT_3D('',#8260,#6724,#6725);
#5702=AXIS2_PLACEMENT_3D('',#8261,#6726,#6727);
#5703=AXIS2_PLACEMENT_3D('',#8262,#6728,#6729);
#5704=AXIS2_PLACEMENT_3D('',#8274,#6731,#6732);
#5705=AXIS2_PLACEMENT_3D('',#8290,#6733,#6734);
#5706=AXIS2_PLACEMENT_3D('',#8292,#6735,#6736);
#5707=AXIS2_PLACEMENT_3D('',#8318,#6738,#6739);
#5708=AXIS2_PLACEMENT_3D('',#8321,#6742,#6743);
#5709=AXIS2_PLACEMENT_3D('',#8323,#6745,#6746);
#5710=AXIS2_PLACEMENT_3D('',#8325,#6748,#6749);
#5711=AXIS2_PLACEMENT_3D('',#8327,#6750,#6751);
#5712=AXIS2_PLACEMENT_3D('',#8330,#6753,#6754);
#5713=AXIS2_PLACEMENT_3D('',#8331,#6755,#6756);
#5714=AXIS2_PLACEMENT_3D('',#8333,#6758,#6759);
#5715=AXIS2_PLACEMENT_3D('',#8335,#6761,#6762);
#5716=AXIS2_PLACEMENT_3D('',#8336,#6763,#6764);
#5717=AXIS2_PLACEMENT_3D('',#8337,#6765,#6766);
#5718=AXIS2_PLACEMENT_3D('',#8338,#6767,#6768);
#5719=AXIS2_PLACEMENT_3D('',#8339,#6769,#6770);
#5720=AXIS2_PLACEMENT_3D('',#8341,#6771,#6772);
#5721=AXIS2_PLACEMENT_3D('',#8344,#6774,#6775);
#5722=AXIS2_PLACEMENT_3D('',#8345,#6776,#6777);
#5723=AXIS2_PLACEMENT_3D('',#8346,#6778,#6779);
#5724=AXIS2_PLACEMENT_3D('',#8348,#6780,#6781);
#5725=AXIS2_PLACEMENT_3D('',#8351,#6783,#6784);
#5726=AXIS2_PLACEMENT_3D('',#8352,#6785,#6786);
#5727=AXIS2_PLACEMENT_3D('',#8353,#6787,#6788);
#5728=AXIS2_PLACEMENT_3D('',#8354,#6789,#6790);
#5729=AXIS2_PLACEMENT_3D('',#8355,#6791,#6792);
#5730=AXIS2_PLACEMENT_3D('',#8357,#6793,#6794);
#5731=AXIS2_PLACEMENT_3D('',#8358,#6795,#6796);
#5732=AXIS2_PLACEMENT_3D('',#8360,#6797,#6798);
#5733=AXIS2_PLACEMENT_3D('',#8362,#6800,#6801);
#5734=AXIS2_PLACEMENT_3D('',#8364,#6802,#6803);
#5735=AXIS2_PLACEMENT_3D('',#8366,#6805,#6806);
#5736=AXIS2_PLACEMENT_3D('',#8367,#6807,#6808);
#5737=AXIS2_PLACEMENT_3D('',#8368,#6809,#6810);
#5738=AXIS2_PLACEMENT_3D('',#8371,#6811,#6812);
#5739=AXIS2_PLACEMENT_3D('',#8373,#6814,#6815);
#5740=AXIS2_PLACEMENT_3D('',#8387,#6819,#6820);
#5741=AXIS2_PLACEMENT_3D('',#8389,#6821,#6822);
#5742=AXIS2_PLACEMENT_3D('',#8393,#6824,#6825);
#5743=AXIS2_PLACEMENT_3D('',#8396,#6827,#6828);
#5744=AXIS2_PLACEMENT_3D('',#8398,#6829,#6830);
#5745=AXIS2_PLACEMENT_3D('',#8401,#6832,#6833);
#5746=AXIS2_PLACEMENT_3D('',#8402,#6834,#6835);
#5747=AXIS2_PLACEMENT_3D('',#8404,#6836,#6837);
#5748=AXIS2_PLACEMENT_3D('',#8408,#6838,#6839);
#5749=AXIS2_PLACEMENT_3D('',#8415,#6842,#6843);
#5750=AXIS2_PLACEMENT_3D('',#8416,#6844,#6845);
#5751=AXIS2_PLACEMENT_3D('',#8417,#6846,#6847);
#5752=AXIS2_PLACEMENT_3D('',#8418,#6848,#6849);
#5753=AXIS2_PLACEMENT_3D('',#8419,#6850,#6851);
#5754=AXIS2_PLACEMENT_3D('',#8420,#6852,#6853);
#5755=AXIS2_PLACEMENT_3D('',#8421,#6854,#6855);
#5756=AXIS2_PLACEMENT_3D('',#8430,#6860,#6861);
#5757=AXIS2_PLACEMENT_3D('',#8436,#6865,#6866);
#5758=AXIS2_PLACEMENT_3D('',#8442,#6870,#6871);
#5759=AXIS2_PLACEMENT_3D('',#8448,#6875,#6876);
#5760=AXIS2_PLACEMENT_3D('',#8454,#6880,#6881);
#5761=AXIS2_PLACEMENT_3D('',#8457,#6884,#6885);
#5762=AXIS2_PLACEMENT_3D('',#8458,#6886,#6887);
#5763=AXIS2_PLACEMENT_3D('',#8459,#6888,#6889);
#5764=AXIS2_PLACEMENT_3D('',#8461,#6890,#6891);
#5765=AXIS2_PLACEMENT_3D('',#8462,#6892,#6893);
#5766=AXIS2_PLACEMENT_3D('',#8464,#6894,#6895);
#5767=AXIS2_PLACEMENT_3D('',#8465,#6896,#6897);
#5768=AXIS2_PLACEMENT_3D('',#8467,#6898,#6899);
#5769=AXIS2_PLACEMENT_3D('',#8469,#6901,#6902);
#5770=AXIS2_PLACEMENT_3D('',#8471,#6903,#6904);
#5771=AXIS2_PLACEMENT_3D('',#8473,#6906,#6907);
#5772=AXIS2_PLACEMENT_3D('',#8475,#6908,#6909);
#5773=AXIS2_PLACEMENT_3D('',#8477,#6911,#6912);
#5774=AXIS2_PLACEMENT_3D('',#8479,#6913,#6914);
#5775=AXIS2_PLACEMENT_3D('',#8480,#6915,#6916);
#5776=AXIS2_PLACEMENT_3D('',#8482,#6917,#6918);
#5777=AXIS2_PLACEMENT_3D('',#8484,#6920,#6921);
#5778=AXIS2_PLACEMENT_3D('',#8486,#6923,#6924);
#5779=AXIS2_PLACEMENT_3D('',#8487,#6925,#6926);
#5780=AXIS2_PLACEMENT_3D('',#8488,#6927,#6928);
#5781=AXIS2_PLACEMENT_3D('',#8490,#6929,#6930);
#5782=AXIS2_PLACEMENT_3D('',#8493,#6932,#6933);
#5783=AXIS2_PLACEMENT_3D('',#8494,#6934,#6935);
#5784=AXIS2_PLACEMENT_3D('',#8496,#6936,#6937);
#5785=AXIS2_PLACEMENT_3D('',#8499,#6939,#6940);
#5786=AXIS2_PLACEMENT_3D('',#8500,#6941,#6942);
#5787=AXIS2_PLACEMENT_3D('',#8505,#6944,#6945);
#5788=AXIS2_PLACEMENT_3D('',#8508,#6947,#6948);
#5789=AXIS2_PLACEMENT_3D('',#8509,#6949,#6950);
#5790=AXIS2_PLACEMENT_3D('',#8513,#6952,#6953);
#5791=AXIS2_PLACEMENT_3D('',#8515,#6955,#6956);
#5792=AXIS2_PLACEMENT_3D('',#8519,#6959,#6960);
#5793=AXIS2_PLACEMENT_3D('',#8522,#6962,#6963);
#5794=AXIS2_PLACEMENT_3D('',#8523,#6964,#6965);
#5795=AXIS2_PLACEMENT_3D('',#8525,#6967,#6968);
#5796=AXIS2_PLACEMENT_3D('',#8527,#6969,#6970);
#5797=AXIS2_PLACEMENT_3D('',#8530,#6972,#6973);
#5798=AXIS2_PLACEMENT_3D('',#8531,#6974,#6975);
#5799=AXIS2_PLACEMENT_3D('',#8533,#6976,#6977);
#5800=AXIS2_PLACEMENT_3D('',#8536,#6979,#6980);
#5801=AXIS2_PLACEMENT_3D('',#8537,#6981,#6982);
#5802=AXIS2_PLACEMENT_3D('',#8546,#6987,#6988);
#5803=AXIS2_PLACEMENT_3D('',#8555,#6993,#6994);
#5804=AXIS2_PLACEMENT_3D('',#8561,#6998,#6999);
#5805=AXIS2_PLACEMENT_3D('',#8564,#7002,#7003);
#5806=AXIS2_PLACEMENT_3D('',#8571,#7006,#7007);
#5807=AXIS2_PLACEMENT_3D('',#8573,#7009,#7010);
#5808=AXIS2_PLACEMENT_3D('',#8579,#7014,#7015);
#5809=AXIS2_PLACEMENT_3D('',#8584,#7018,#7019);
#5810=AXIS2_PLACEMENT_3D('',#8585,#7020,#7021);
#5811=AXIS2_PLACEMENT_3D('',#8588,#7024,#7025);
#5812=AXIS2_PLACEMENT_3D('',#8590,#7026,#7027);
#5813=AXIS2_PLACEMENT_3D('',#8593,#7029,#7030);
#5814=AXIS2_PLACEMENT_3D('',#8594,#7031,#7032);
#5815=AXIS2_PLACEMENT_3D('',#8595,#7033,#7034);
#5816=AXIS2_PLACEMENT_3D('',#8596,#7035,#7036);
#5817=AXIS2_PLACEMENT_3D('',#8604,#7041,#7042);
#5818=AXIS2_PLACEMENT_3D('',#8608,#7045,#7046);
#5819=AXIS2_PLACEMENT_3D('',#8612,#7049,#7050);
#5820=AXIS2_PLACEMENT_3D('',#8616,#7053,#7054);
#5821=AXIS2_PLACEMENT_3D('',#8618,#7056,#7057);
#5822=AXIS2_PLACEMENT_3D('',#8619,#7058,#7059);
#5823=AXIS2_PLACEMENT_3D('',#8620,#7060,#7061);
#5824=AXIS2_PLACEMENT_3D('',#8622,#7062,#7063);
#5825=AXIS2_PLACEMENT_3D('',#8625,#7065,#7066);
#5826=AXIS2_PLACEMENT_3D('',#8626,#7067,#7068);
#5827=AXIS2_PLACEMENT_3D('',#8627,#7069,#7070);
#5828=AXIS2_PLACEMENT_3D('',#8629,#7071,#7072);
#5829=AXIS2_PLACEMENT_3D('',#8632,#7074,#7075);
#5830=AXIS2_PLACEMENT_3D('',#8633,#7076,#7077);
#5831=AXIS2_PLACEMENT_3D('',#8634,#7078,#7079);
#5832=AXIS2_PLACEMENT_3D('',#8635,#7080,#7081);
#5833=AXIS2_PLACEMENT_3D('',#8636,#7082,#7083);
#5834=AXIS2_PLACEMENT_3D('',#8645,#7088,#7089);
#5835=AXIS2_PLACEMENT_3D('',#8651,#7093,#7094);
#5836=AXIS2_PLACEMENT_3D('',#8657,#7098,#7099);
#5837=AXIS2_PLACEMENT_3D('',#8663,#7103,#7104);
#5838=AXIS2_PLACEMENT_3D('',#8669,#7108,#7109);
#5839=AXIS2_PLACEMENT_3D('',#8672,#7112,#7113);
#5840=AXIS2_PLACEMENT_3D('',#8673,#7114,#7115);
#5841=AXIS2_PLACEMENT_3D('',#8674,#7116,#7117);
#5842=AXIS2_PLACEMENT_3D('',#8676,#7118,#7119);
#5843=AXIS2_PLACEMENT_3D('',#8677,#7120,#7121);
#5844=AXIS2_PLACEMENT_3D('',#8679,#7122,#7123);
#5845=AXIS2_PLACEMENT_3D('',#8680,#7124,#7125);
#5846=AXIS2_PLACEMENT_3D('',#8682,#7126,#7127);
#5847=AXIS2_PLACEMENT_3D('',#8684,#7129,#7130);
#5848=AXIS2_PLACEMENT_3D('',#8686,#7131,#7132);
#5849=AXIS2_PLACEMENT_3D('',#8688,#7134,#7135);
#5850=AXIS2_PLACEMENT_3D('',#8690,#7136,#7137);
#5851=AXIS2_PLACEMENT_3D('',#8692,#7139,#7140);
#5852=AXIS2_PLACEMENT_3D('',#8694,#7141,#7142);
#5853=AXIS2_PLACEMENT_3D('',#8695,#7143,#7144);
#5854=AXIS2_PLACEMENT_3D('',#8697,#7145,#7146);
#5855=AXIS2_PLACEMENT_3D('',#8699,#7148,#7149);
#5856=AXIS2_PLACEMENT_3D('',#8701,#7151,#7152);
#5857=AXIS2_PLACEMENT_3D('',#8702,#7153,#7154);
#5858=AXIS2_PLACEMENT_3D('',#8703,#7155,#7156);
#5859=AXIS2_PLACEMENT_3D('',#8705,#7157,#7158);
#5860=AXIS2_PLACEMENT_3D('',#8708,#7160,#7161);
#5861=AXIS2_PLACEMENT_3D('',#8709,#7162,#7163);
#5862=AXIS2_PLACEMENT_3D('',#8711,#7164,#7165);
#5863=AXIS2_PLACEMENT_3D('',#8714,#7167,#7168);
#5864=AXIS2_PLACEMENT_3D('',#8715,#7169,#7170);
#5865=AXIS2_PLACEMENT_3D('',#8720,#7172,#7173);
#5866=AXIS2_PLACEMENT_3D('',#8723,#7175,#7176);
#5867=AXIS2_PLACEMENT_3D('',#8724,#7177,#7178);
#5868=AXIS2_PLACEMENT_3D('',#8730,#7182,#7183);
#5869=AXIS2_PLACEMENT_3D('',#8733,#7185,#7186);
#5870=AXIS2_PLACEMENT_3D('',#8734,#7187,#7188);
#5871=AXIS2_PLACEMENT_3D('',#8738,#7191,#7192);
#5872=AXIS2_PLACEMENT_3D('',#8739,#7193,#7194);
#5873=AXIS2_PLACEMENT_3D('',#8740,#7195,#7196);
#5874=AXIS2_PLACEMENT_3D('',#8741,#7197,#7198);
#5875=AXIS2_PLACEMENT_3D('',#8742,#7199,#7200);
#5876=AXIS2_PLACEMENT_3D('',#8743,#7201,#7202);
#5877=AXIS2_PLACEMENT_3D('',#8744,#7203,#7204);
#5878=AXIS2_PLACEMENT_3D('',#8746,#7205,#7206);
#5879=AXIS2_PLACEMENT_3D('',#8749,#7208,#7209);
#5880=AXIS2_PLACEMENT_3D('',#8750,#7210,#7211);
#5881=AXIS2_PLACEMENT_3D('',#8751,#7212,#7213);
#5882=AXIS2_PLACEMENT_3D('',#8753,#7214,#7215);
#5883=AXIS2_PLACEMENT_3D('',#8756,#7217,#7218);
#5884=AXIS2_PLACEMENT_3D('',#8757,#7219,#7220);
#5885=AXIS2_PLACEMENT_3D('',#8759,#7221,#7222);
#5886=AXIS2_PLACEMENT_3D('',#8762,#7224,#7225);
#5887=AXIS2_PLACEMENT_3D('',#8763,#7226,#7227);
#5888=AXIS2_PLACEMENT_3D('',#8772,#7232,#7233);
#5889=AXIS2_PLACEMENT_3D('',#8781,#7238,#7239);
#5890=AXIS2_PLACEMENT_3D('',#8792,#7246,#7247);
#5891=AXIS2_PLACEMENT_3D('',#8798,#7251,#7252);
#5892=AXIS2_PLACEMENT_3D('',#8802,#7255,#7256);
#5893=AXIS2_PLACEMENT_3D('',#8805,#7258,#7259);
#5894=AXIS2_PLACEMENT_3D('',#8806,#7260,#7261);
#5895=AXIS2_PLACEMENT_3D('',#8811,#7265,#7266);
#5896=AXIS2_PLACEMENT_3D('',#8812,#7267,#7268);
#5897=AXIS2_PLACEMENT_3D('',#8814,#7270,#7271);
#5898=AXIS2_PLACEMENT_3D('',#8815,#7272,#7273);
#5899=AXIS2_PLACEMENT_3D('',#8817,#7274,#7275);
#5900=AXIS2_PLACEMENT_3D('',#8819,#7277,#7278);
#5901=AXIS2_PLACEMENT_3D('',#8820,#7279,#7280);
#5902=AXIS2_PLACEMENT_3D('',#8821,#7281,#7282);
#5903=AXIS2_PLACEMENT_3D('',#8823,#7283,#7284);
#5904=AXIS2_PLACEMENT_3D('',#8826,#7286,#7287);
#5905=AXIS2_PLACEMENT_3D('',#8827,#7288,#7289);
#5906=AXIS2_PLACEMENT_3D('',#8829,#7290,#7291);
#5907=AXIS2_PLACEMENT_3D('',#8831,#7293,#7294);
#5908=AXIS2_PLACEMENT_3D('',#8832,#7295,#7296);
#5909=AXIS2_PLACEMENT_3D('',#8834,#7297,#7298);
#5910=AXIS2_PLACEMENT_3D('',#8860,#7300,#7301);
#5911=AXIS2_PLACEMENT_3D('',#8866,#7305,#7306);
#5912=AXIS2_PLACEMENT_3D('',#8870,#7309,#7310);
#5913=AXIS2_PLACEMENT_3D('',#8874,#7313,#7314);
#5914=AXIS2_PLACEMENT_3D('',#8878,#7317,#7318);
#5915=AXIS2_PLACEMENT_3D('',#8882,#7321,#7322);
#5916=AXIS2_PLACEMENT_3D('',#8884,#7324,#7325);
#5917=AXIS2_PLACEMENT_3D('',#8885,#7326,#7327);
#5918=AXIS2_PLACEMENT_3D('',#8886,#7328,#7329);
#5919=AXIS2_PLACEMENT_3D('',#8887,#7330,#7331);
#5920=AXIS2_PLACEMENT_3D('',#8899,#7333,#7334);
#5921=AXIS2_PLACEMENT_3D('',#8915,#7335,#7336);
#5922=AXIS2_PLACEMENT_3D('',#8917,#7337,#7338);
#5923=AXIS2_PLACEMENT_3D('',#8943,#7340,#7341);
#5924=AXIS2_PLACEMENT_3D('',#8946,#7344,#7345);
#5925=AXIS2_PLACEMENT_3D('',#8948,#7347,#7348);
#5926=AXIS2_PLACEMENT_3D('',#8950,#7350,#7351);
#5927=AXIS2_PLACEMENT_3D('',#8952,#7352,#7353);
#5928=AXIS2_PLACEMENT_3D('',#8955,#7355,#7356);
#5929=AXIS2_PLACEMENT_3D('',#8956,#7357,#7358);
#5930=AXIS2_PLACEMENT_3D('',#8958,#7360,#7361);
#5931=AXIS2_PLACEMENT_3D('',#8960,#7363,#7364);
#5932=AXIS2_PLACEMENT_3D('',#8961,#7365,#7366);
#5933=AXIS2_PLACEMENT_3D('',#8962,#7367,#7368);
#5934=AXIS2_PLACEMENT_3D('',#8963,#7369,#7370);
#5935=AXIS2_PLACEMENT_3D('',#8964,#7371,#7372);
#5936=AXIS2_PLACEMENT_3D('',#8966,#7373,#7374);
#5937=AXIS2_PLACEMENT_3D('',#8969,#7376,#7377);
#5938=AXIS2_PLACEMENT_3D('',#8970,#7378,#7379);
#5939=AXIS2_PLACEMENT_3D('',#8971,#7380,#7381);
#5940=AXIS2_PLACEMENT_3D('',#8972,#7382,#7383);
#5941=AXIS2_PLACEMENT_3D('',#8973,#7384,#7385);
#5942=AXIS2_PLACEMENT_3D('',#9051,#7387,#7388);
#5943=AXIS2_PLACEMENT_3D('',#9053,#7389,#7390);
#5944=AXIS2_PLACEMENT_3D('',#9054,#7391,#7392);
#5945=AXIS2_PLACEMENT_3D('',#9056,#7393,#7394);
#5946=AXIS2_PLACEMENT_3D('',#9058,#7396,#7397);
#5947=AXIS2_PLACEMENT_3D('',#9060,#7398,#7399);
#5948=AXIS2_PLACEMENT_3D('',#9062,#7401,#7402);
#5949=AXIS2_PLACEMENT_3D('',#9064,#7403,#7404);
#5950=AXIS2_PLACEMENT_3D('',#9065,#7405,#7406);
#5951=AXIS2_PLACEMENT_3D('',#9067,#7407,#7408);
#5952=AXIS2_PLACEMENT_3D('',#9070,#7411,#7412);
#5953=AXIS2_PLACEMENT_3D('',#9072,#7413,#7414);
#5954=AXIS2_PLACEMENT_3D('',#9074,#7416,#7417);
#5955=AXIS2_PLACEMENT_3D('',#9075,#7418,#7419);
#5956=AXIS2_PLACEMENT_3D('',#9076,#7420,#7421);
#5957=AXIS2_PLACEMENT_3D('',#9078,#7422,#7423);
#5958=AXIS2_PLACEMENT_3D('',#9081,#7425,#7426);
#5959=AXIS2_PLACEMENT_3D('',#9082,#7427,#7428);
#5960=AXIS2_PLACEMENT_3D('',#9084,#7429,#7430);
#5961=AXIS2_PLACEMENT_3D('',#9087,#7432,#7433);
#5962=AXIS2_PLACEMENT_3D('',#9088,#7434,#7435);
#5963=AXIS2_PLACEMENT_3D('',#9089,#7436,#7437);
#5964=AXIS2_PLACEMENT_3D('',#9090,#7438,#7439);
#5965=AXIS2_PLACEMENT_3D('',#9091,#7440,#7441);
#5966=AXIS2_PLACEMENT_3D('',#9093,#7442,#7443);
#5967=AXIS2_PLACEMENT_3D('',#9096,#7445,#7446);
#5968=AXIS2_PLACEMENT_3D('',#9097,#7447,#7448);
#5969=AXIS2_PLACEMENT_3D('',#9099,#7449,#7450);
#5970=AXIS2_PLACEMENT_3D('',#9102,#7452,#7453);
#5971=AXIS2_PLACEMENT_3D('',#9103,#7454,#7455);
#5972=AXIS2_PLACEMENT_3D('',#9104,#7456,#7457);
#5973=AXIS2_PLACEMENT_3D('',#9105,#7458,#7459);
#5974=AXIS2_PLACEMENT_3D('',#9106,#7460,#7461);
#5975=AXIS2_PLACEMENT_3D('',#9108,#7462,#7463);
#5976=AXIS2_PLACEMENT_3D('',#9109,#7464,#7465);
#5977=AXIS2_PLACEMENT_3D('',#9164,#7466,#7467);
#5978=AXIS2_PLACEMENT_3D('',#9167,#7468,#7469);
#5979=AXIS2_PLACEMENT_3D('',#9169,#7471,#7472);
#5980=AXIS2_PLACEMENT_3D('',#9175,#7476,#7477);
#5981=AXIS2_PLACEMENT_3D('',#9177,#7478,#7479);
#5982=AXIS2_PLACEMENT_3D('',#9179,#7481,#7482);
#5983=AXIS2_PLACEMENT_3D('',#9180,#7483,#7484);
#5984=AXIS2_PLACEMENT_3D('',#9181,#7485,#7486);
#5985=AXIS2_PLACEMENT_3D('',#9182,#7487,#7488);
#5986=AXIS2_PLACEMENT_3D('',#9183,#7489,#7490);
#5987=AXIS2_PLACEMENT_3D('',#9184,#7491,#7492);
#5988=AXIS2_PLACEMENT_3D('',#9185,#7493,#7494);
#5989=AXIS2_PLACEMENT_3D('',#9186,#7495,#7496);
#5990=AXIS2_PLACEMENT_3D('',#9187,#7497,#7498);
#5991=AXIS2_PLACEMENT_3D('',#9188,#7499,#7500);
#5992=AXIS2_PLACEMENT_3D('',#9189,#7501,#7502);
#5993=AXIS2_PLACEMENT_3D('',#9190,#7503,#7504);
#5994=AXIS2_PLACEMENT_3D('',#9191,#7505,#7506);
#5995=AXIS2_PLACEMENT_3D('',#9192,#7507,#7508);
#5996=AXIS2_PLACEMENT_3D('',#9193,#7509,#7510);
#5997=AXIS2_PLACEMENT_3D('',#9194,#7511,#7512);
#5998=AXIS2_PLACEMENT_3D('',#9195,#7513,#7514);
#5999=AXIS2_PLACEMENT_3D('',#9196,#7515,#7516);
#6000=AXIS2_PLACEMENT_3D('',#9197,#7517,#7518);
#6001=AXIS2_PLACEMENT_3D('',#9198,#7519,#7520);
#6002=AXIS2_PLACEMENT_3D('',#9199,#7521,#7522);
#6003=AXIS2_PLACEMENT_3D('',#9200,#7523,#7524);
#6004=AXIS2_PLACEMENT_3D('',#9201,#7525,#7526);
#6005=AXIS2_PLACEMENT_3D('',#9202,#7527,#7528);
#6006=AXIS2_PLACEMENT_3D('',#9203,#7529,#7530);
#6007=AXIS2_PLACEMENT_3D('',#9204,#7531,#7532);
#6008=AXIS2_PLACEMENT_3D('',#9205,#7533,#7534);
#6009=AXIS2_PLACEMENT_3D('',#9206,#7535,#7536);
#6010=AXIS2_PLACEMENT_3D('',#9207,#7537,#7538);
#6011=AXIS2_PLACEMENT_3D('',#9208,#7539,#7540);
#6012=AXIS2_PLACEMENT_3D('',#9209,#7541,#7542);
#6013=AXIS2_PLACEMENT_3D('',#9210,#7543,#7544);
#6014=AXIS2_PLACEMENT_3D('',#9211,#7545,#7546);
#6015=AXIS2_PLACEMENT_3D('',#9212,#7547,#7548);
#6016=AXIS2_PLACEMENT_3D('',#9213,#7549,#7550);
#6017=AXIS2_PLACEMENT_3D('',#9214,#7551,#7552);
#6018=AXIS2_PLACEMENT_3D('',#9215,#7553,#7554);
#6019=AXIS2_PLACEMENT_3D('',#9216,#7555,#7556);
#6020=AXIS2_PLACEMENT_3D('',#9217,#7557,#7558);
#6021=AXIS2_PLACEMENT_3D('',#9218,#7559,#7560);
#6022=AXIS2_PLACEMENT_3D('',#9219,#7561,#7562);
#6023=AXIS2_PLACEMENT_3D('',#9220,#7563,#7564);
#6024=AXIS2_PLACEMENT_3D('',#9221,#7565,#7566);
#6025=AXIS2_PLACEMENT_3D('',#9222,#7567,#7568);
#6026=AXIS2_PLACEMENT_3D('',#9223,#7569,#7570);
#6027=AXIS2_PLACEMENT_3D('',#9224,#7571,#7572);
#6028=AXIS2_PLACEMENT_3D('',#9225,#7573,#7574);
#6029=DIRECTION('axis',(0.,0.,1.));
#6030=DIRECTION('refdir',(1.,0.,0.));
#6031=DIRECTION('axis',(0.,0.,1.));
#6032=DIRECTION('refdir',(1.,0.,0.));
#6033=DIRECTION('axis',(0.,0.,1.));
#6034=DIRECTION('refdir',(1.,0.,0.));
#6035=DIRECTION('center_axis',(0.,1.,0.));
#6036=DIRECTION('ref_axis',(1.,0.,0.));
#6037=DIRECTION('',(0.,1.,0.));
#6038=DIRECTION('center_axis',(0.,1.,0.));
#6039=DIRECTION('ref_axis',(1.,0.,0.));
#6040=DIRECTION('',(0.,1.,0.));
#6041=DIRECTION('center_axis',(0.,1.,0.));
#6042=DIRECTION('ref_axis',(1.,0.,0.));
#6043=DIRECTION('',(0.,-1.,0.));
#6044=DIRECTION('center_axis',(0.,1.,0.));
#6045=DIRECTION('ref_axis',(1.,0.,0.));
#6046=DIRECTION('center_axis',(0.,1.,0.));
#6047=DIRECTION('ref_axis',(1.,0.,0.));
#6048=DIRECTION('center_axis',(0.,1.,0.));
#6049=DIRECTION('ref_axis',(1.,0.,0.));
#6050=DIRECTION('center_axis',(0.,1.,0.));
#6051=DIRECTION('ref_axis',(-1.,0.,0.));
#6052=DIRECTION('',(1.,0.,0.));
#6053=DIRECTION('',(0.,0.,-1.));
#6054=DIRECTION('',(-1.,0.,0.));
#6055=DIRECTION('',(0.,0.,1.));
#6056=DIRECTION('',(-1.,0.,0.));
#6057=DIRECTION('',(0.,0.,1.));
#6058=DIRECTION('',(-1.,0.,0.));
#6059=DIRECTION('',(0.,0.,1.));
#6060=DIRECTION('',(-1.,0.,0.));
#6061=DIRECTION('center_axis',(0.,0.,-1.));
#6062=DIRECTION('ref_axis',(-1.,0.,0.));
#6063=DIRECTION('',(0.,1.,0.));
#6064=DIRECTION('',(1.,0.,0.));
#6065=DIRECTION('center_axis',(0.,0.,1.));
#6066=DIRECTION('ref_axis',(1.,0.,0.));
#6067=DIRECTION('',(-1.,0.,0.));
#6068=DIRECTION('',(0.,1.,0.));
#6069=DIRECTION('center_axis',(1.,0.,0.));
#6070=DIRECTION('ref_axis',(0.,0.,-1.));
#6071=DIRECTION('',(0.,0.,1.));
#6072=DIRECTION('',(0.,-1.,0.));
#6073=DIRECTION('center_axis',(-1.,0.,0.));
#6074=DIRECTION('ref_axis',(0.,0.,1.));
#6075=DIRECTION('',(0.,1.,0.));
#6076=DIRECTION('',(0.,0.,-1.));
#6077=DIRECTION('center_axis',(0.,1.,0.));
#6078=DIRECTION('ref_axis',(1.,0.,0.));
#6079=DIRECTION('',(-1.,0.,0.));
#6080=DIRECTION('center_axis',(0.,0.,1.));
#6081=DIRECTION('ref_axis',(1.,0.,0.));
#6082=DIRECTION('',(0.,-1.,0.));
#6083=DIRECTION('',(1.,0.,0.));
#6084=DIRECTION('',(0.,1.,0.));
#6085=DIRECTION('',(0.,-1.,0.));
#6086=DIRECTION('',(-1.,0.,0.));
#6087=DIRECTION('',(0.,1.,0.));
#6088=DIRECTION('',(1.,0.,0.));
#6089=DIRECTION('',(0.,-1.,0.));
#6090=DIRECTION('',(-1.,0.,0.));
#6091=DIRECTION('',(0.,1.,0.));
#6092=DIRECTION('',(1.,0.,0.));
#6093=DIRECTION('',(0.,-1.,0.));
#6094=DIRECTION('',(-1.,0.,0.));
#6095=DIRECTION('',(0.,1.,0.));
#6096=DIRECTION('',(1.,0.,0.));
#6097=DIRECTION('center_axis',(0.,0.,-1.));
#6098=DIRECTION('ref_axis',(1.,0.,0.));
#6099=DIRECTION('center_axis',(0.,0.,-1.));
#6100=DIRECTION('ref_axis',(1.,0.,0.));
#6101=DIRECTION('center_axis',(0.,0.,1.));
#6102=DIRECTION('ref_axis',(1.,0.,0.));
#6103=DIRECTION('center_axis',(0.,0.,1.));
#6104=DIRECTION('ref_axis',(1.,0.,0.));
#6105=DIRECTION('',(0.,0.,1.));
#6106=DIRECTION('center_axis',(0.,0.,1.));
#6107=DIRECTION('ref_axis',(1.,0.,0.));
#6108=DIRECTION('center_axis',(0.,0.,1.));
#6109=DIRECTION('ref_axis',(1.,0.,0.));
#6110=DIRECTION('',(0.,0.,1.));
#6111=DIRECTION('center_axis',(1.,0.,0.));
#6112=DIRECTION('ref_axis',(0.,0.,-1.));
#6113=DIRECTION('center_axis',(1.,0.,0.));
#6114=DIRECTION('ref_axis',(0.,0.,-1.));
#6115=DIRECTION('',(1.,0.,0.));
#6116=DIRECTION('center_axis',(-1.,0.,0.));
#6117=DIRECTION('ref_axis',(0.,0.,-1.));
#6118=DIRECTION('center_axis',(0.,1.,0.));
#6119=DIRECTION('ref_axis',(1.,0.,0.));
#6120=DIRECTION('',(0.,0.,1.));
#6121=DIRECTION('',(-1.,0.,0.));
#6122=DIRECTION('',(0.,0.,-1.));
#6123=DIRECTION('center_axis',(1.,0.,0.));
#6124=DIRECTION('ref_axis',(0.,0.,-1.));
#6125=DIRECTION('',(0.,0.,-1.));
#6126=DIRECTION('',(0.,1.,0.));
#6127=DIRECTION('center_axis',(-1.,0.,0.));
#6128=DIRECTION('ref_axis',(0.,0.,1.));
#6129=DIRECTION('',(0.,1.,0.));
#6130=DIRECTION('',(0.,0.,1.));
#6131=DIRECTION('center_axis',(0.,0.,1.));
#6132=DIRECTION('ref_axis',(1.,0.,0.));
#6133=DIRECTION('',(1.,0.,0.));
#6134=DIRECTION('center_axis',(0.,1.,0.));
#6135=DIRECTION('ref_axis',(0.,0.,1.));
#6136=DIRECTION('center_axis',(0.,1.,0.));
#6137=DIRECTION('ref_axis',(1.,0.,0.));
#6138=DIRECTION('center_axis',(0.,1.,0.));
#6139=DIRECTION('ref_axis',(1.,0.,0.));
#6140=DIRECTION('',(0.,1.,0.));
#6141=DIRECTION('center_axis',(0.,-1.,0.));
#6142=DIRECTION('ref_axis',(1.,0.,0.));
#6143=DIRECTION('center_axis',(0.,1.,0.));
#6144=DIRECTION('ref_axis',(1.,0.,0.));
#6145=DIRECTION('center_axis',(0.,1.,0.));
#6146=DIRECTION('ref_axis',(1.,0.,0.));
#6147=DIRECTION('',(0.,1.,0.));
#6148=DIRECTION('center_axis',(0.,-1.,0.));
#6149=DIRECTION('ref_axis',(1.,0.,0.));
#6150=DIRECTION('center_axis',(0.,1.,0.));
#6151=DIRECTION('ref_axis',(1.,0.,0.));
#6152=DIRECTION('',(0.,0.,1.));
#6153=DIRECTION('',(-1.,0.,0.));
#6154=DIRECTION('',(0.,0.,-1.));
#6155=DIRECTION('center_axis',(1.,0.,0.));
#6156=DIRECTION('ref_axis',(0.,0.,-1.));
#6157=DIRECTION('',(0.,0.,-1.));
#6158=DIRECTION('',(0.,1.,0.));
#6159=DIRECTION('center_axis',(-1.,0.,0.));
#6160=DIRECTION('ref_axis',(0.,0.,1.));
#6161=DIRECTION('',(0.,1.,0.));
#6162=DIRECTION('',(0.,0.,1.));
#6163=DIRECTION('center_axis',(0.,0.,1.));
#6164=DIRECTION('ref_axis',(1.,0.,0.));
#6165=DIRECTION('',(1.,0.,0.));
#6166=DIRECTION('center_axis',(0.,1.,0.));
#6167=DIRECTION('ref_axis',(0.,0.,1.));
#6168=DIRECTION('center_axis',(0.,1.,0.));
#6169=DIRECTION('ref_axis',(1.,0.,0.));
#6170=DIRECTION('',(0.,0.,1.));
#6171=DIRECTION('',(-1.,0.,0.));
#6172=DIRECTION('',(0.,0.,-1.));
#6173=DIRECTION('center_axis',(1.,0.,0.));
#6174=DIRECTION('ref_axis',(0.,0.,-1.));
#6175=DIRECTION('',(0.,0.,-1.));
#6176=DIRECTION('',(0.,1.,0.));
#6177=DIRECTION('center_axis',(-1.,0.,0.));
#6178=DIRECTION('ref_axis',(0.,0.,1.));
#6179=DIRECTION('',(0.,1.,0.));
#6180=DIRECTION('',(0.,0.,1.));
#6181=DIRECTION('center_axis',(0.,0.,1.));
#6182=DIRECTION('ref_axis',(1.,0.,0.));
#6183=DIRECTION('',(1.,0.,0.));
#6184=DIRECTION('center_axis',(0.,1.,0.));
#6185=DIRECTION('ref_axis',(0.,0.,1.));
#6186=DIRECTION('center_axis',(1.,0.,0.));
#6187=DIRECTION('ref_axis',(0.,1.,0.));
#6188=DIRECTION('',(0.,1.,0.));
#6189=DIRECTION('',(0.,0.,1.));
#6190=DIRECTION('center_axis',(0.,-1.,0.));
#6191=DIRECTION('ref_axis',(1.,0.,0.));
#6192=DIRECTION('',(1.,0.,0.));
#6193=DIRECTION('',(0.,0.,1.));
#6194=DIRECTION('center_axis',(-1.,0.,0.));
#6195=DIRECTION('ref_axis',(0.,-1.,0.));
#6196=DIRECTION('',(0.,-1.,0.));
#6197=DIRECTION('center_axis',(0.,0.,1.));
#6198=DIRECTION('ref_axis',(1.,0.,0.));
#6199=DIRECTION('axis',(0.,0.,1.));
#6200=DIRECTION('refdir',(1.,0.,0.));
#6201=DIRECTION('center_axis',(1.,0.,0.));
#6202=DIRECTION('ref_axis',(0.,0.,-1.));
#6203=DIRECTION('',(1.,0.,0.));
#6204=DIRECTION('center_axis',(1.,0.,0.));
#6205=DIRECTION('ref_axis',(0.,0.,-1.));
#6206=DIRECTION('',(-1.,0.,0.));
#6207=DIRECTION('center_axis',(1.,0.,0.));
#6208=DIRECTION('ref_axis',(0.,0.,-1.));
#6209=DIRECTION('center_axis',(1.,0.,0.));
#6210=DIRECTION('ref_axis',(0.,0.,-1.));
#6211=DIRECTION('',(0.,1.,0.));
#6212=DIRECTION('center_axis',(1.,0.,0.));
#6213=DIRECTION('ref_axis',(0.,0.,-1.));
#6214=DIRECTION('',(0.,1.,0.));
#6215=DIRECTION('',(0.,0.,-1.));
#6216=DIRECTION('',(0.,-1.,0.));
#6217=DIRECTION('',(0.,0.,1.));
#6218=DIRECTION('',(0.,1.,0.));
#6219=DIRECTION('center_axis',(1.,0.,0.));
#6220=DIRECTION('ref_axis',(0.,0.,-1.));
#6221=DIRECTION('center_axis',(1.,0.,0.));
#6222=DIRECTION('ref_axis',(0.,0.,-1.));
#6223=DIRECTION('center_axis',(1.,0.,0.));
#6224=DIRECTION('ref_axis',(0.,0.,-1.));
#6225=DIRECTION('',(1.,0.,0.));
#6226=DIRECTION('center_axis',(-1.,0.,0.));
#6227=DIRECTION('ref_axis',(0.,0.,-1.));
#6228=DIRECTION('center_axis',(1.,0.,0.));
#6229=DIRECTION('ref_axis',(0.,0.,-1.));
#6230=DIRECTION('',(1.,0.,0.));
#6231=DIRECTION('center_axis',(-1.,0.,0.));
#6232=DIRECTION('ref_axis',(0.,0.,-1.));
#6233=DIRECTION('center_axis',(0.,0.,1.));
#6234=DIRECTION('ref_axis',(1.,0.,0.));
#6235=DIRECTION('',(-1.,0.,0.));
#6236=DIRECTION('',(0.,-1.,0.));
#6237=DIRECTION('',(1.,0.,0.));
#6238=DIRECTION('center_axis',(0.,0.,1.));
#6239=DIRECTION('ref_axis',(1.,0.,0.));
#6240=DIRECTION('center_axis',(0.,0.,1.));
#6241=DIRECTION('ref_axis',(1.,0.,0.));
#6242=DIRECTION('',(0.,0.,1.));
#6243=DIRECTION('center_axis',(0.,0.,-1.));
#6244=DIRECTION('ref_axis',(1.,0.,0.));
#6245=DIRECTION('center_axis',(0.,0.,1.));
#6246=DIRECTION('ref_axis',(1.,0.,0.));
#6247=DIRECTION('center_axis',(1.,0.,0.));
#6248=DIRECTION('ref_axis',(0.,1.,0.));
#6249=DIRECTION('',(0.,0.,1.));
#6250=DIRECTION('',(0.,1.,0.));
#6251=DIRECTION('',(0.,0.,1.));
#6252=DIRECTION('center_axis',(-1.,0.,0.));
#6253=DIRECTION('ref_axis',(0.,-1.,0.));
#6254=DIRECTION('',(0.,1.,0.));
#6255=DIRECTION('',(0.,0.,1.));
#6256=DIRECTION('',(0.,-1.,0.));
#6257=DIRECTION('',(0.,0.,1.));
#6258=DIRECTION('center_axis',(0.,0.,1.));
#6259=DIRECTION('ref_axis',(1.,0.,0.));
#6260=DIRECTION('',(1.,0.,0.));
#6261=DIRECTION('',(-1.,0.,0.));
#6262=DIRECTION('center_axis',(0.,0.,1.));
#6263=DIRECTION('ref_axis',(1.,0.,0.));
#6264=DIRECTION('',(-1.,0.,0.));
#6265=DIRECTION('',(0.,-1.,0.));
#6266=DIRECTION('',(1.,0.,0.));
#6267=DIRECTION('center_axis',(0.,0.,1.));
#6268=DIRECTION('ref_axis',(1.,0.,0.));
#6269=DIRECTION('center_axis',(0.,0.,1.));
#6270=DIRECTION('ref_axis',(1.,0.,0.));
#6271=DIRECTION('',(0.,0.,1.));
#6272=DIRECTION('center_axis',(0.,0.,-1.));
#6273=DIRECTION('ref_axis',(1.,0.,0.));
#6274=DIRECTION('center_axis',(0.,0.,1.));
#6275=DIRECTION('ref_axis',(1.,0.,0.));
#6276=DIRECTION('center_axis',(1.,0.,0.));
#6277=DIRECTION('ref_axis',(0.,1.,0.));
#6278=DIRECTION('',(0.,0.,1.));
#6279=DIRECTION('',(0.,1.,0.));
#6280=DIRECTION('',(0.,0.,1.));
#6281=DIRECTION('center_axis',(-1.,0.,0.));
#6282=DIRECTION('ref_axis',(0.,-1.,0.));
#6283=DIRECTION('',(0.,1.,0.));
#6284=DIRECTION('',(0.,0.,1.));
#6285=DIRECTION('',(0.,-1.,0.));
#6286=DIRECTION('',(0.,0.,1.));
#6287=DIRECTION('center_axis',(0.,0.,1.));
#6288=DIRECTION('ref_axis',(1.,0.,0.));
#6289=DIRECTION('',(1.,0.,0.));
#6290=DIRECTION('',(-1.,0.,0.));
#6291=DIRECTION('center_axis',(0.,0.,1.));
#6292=DIRECTION('ref_axis',(1.,0.,0.));
#6293=DIRECTION('',(-1.,0.,0.));
#6294=DIRECTION('',(0.,-1.,0.));
#6295=DIRECTION('',(1.,0.,0.));
#6296=DIRECTION('center_axis',(0.,0.,1.));
#6297=DIRECTION('ref_axis',(0.,-1.,0.));
#6298=DIRECTION('',(1.,0.,0.));
#6299=DIRECTION('',(0.,-1.,0.));
#6300=DIRECTION('',(1.,0.,0.));
#6301=DIRECTION('center_axis',(1.,0.,0.));
#6302=DIRECTION('ref_axis',(0.,0.,-1.));
#6303=DIRECTION('',(0.,0.,-1.));
#6304=DIRECTION('',(0.,1.,0.));
#6305=DIRECTION('',(0.,0.,1.));
#6306=DIRECTION('center_axis',(0.,1.,0.));
#6307=DIRECTION('ref_axis',(-1.,0.,0.));
#6308=DIRECTION('',(1.,0.,0.));
#6309=DIRECTION('',(0.,0.,1.));
#6310=DIRECTION('center_axis',(0.,-1.,0.));
#6311=DIRECTION('ref_axis',(1.,0.,0.));
#6312=DIRECTION('',(1.,0.,0.));
#6313=DIRECTION('',(0.,0.,1.));
#6314=DIRECTION('center_axis',(-1.,0.,0.));
#6315=DIRECTION('ref_axis',(0.,-1.,0.));
#6316=DIRECTION('',(0.,-1.,0.));
#6317=DIRECTION('center_axis',(0.,0.,1.));
#6318=DIRECTION('ref_axis',(1.,0.,0.));
#6319=DIRECTION('axis',(0.,0.,1.));
#6320=DIRECTION('refdir',(1.,0.,0.));
#6321=DIRECTION('center_axis',(0.,1.,0.));
#6322=DIRECTION('ref_axis',(1.,0.,0.));
#6323=DIRECTION('center_axis',(0.,1.,0.));
#6324=DIRECTION('ref_axis',(1.,0.,0.));
#6325=DIRECTION('',(0.707106781186548,-0.707106781186547,-8.65956056235494E-17));
#6326=DIRECTION('center_axis',(0.,-1.,0.));
#6327=DIRECTION('ref_axis',(1.,0.,0.));
#6328=DIRECTION('center_axis',(0.,1.,0.));
#6329=DIRECTION('ref_axis',(1.,0.,0.));
#6330=DIRECTION('',(0.,-1.,0.));
#6331=DIRECTION('center_axis',(0.,-1.,0.));
#6332=DIRECTION('ref_axis',(1.,0.,0.));
#6333=DIRECTION('center_axis',(0.,1.,0.));
#6334=DIRECTION('ref_axis',(1.,0.,0.));
#6335=DIRECTION('center_axis',(0.,1.,0.));
#6336=DIRECTION('ref_axis',(1.,0.,0.));
#6337=DIRECTION('center_axis',(0.,1.,0.));
#6338=DIRECTION('ref_axis',(1.,0.,0.));
#6339=DIRECTION('',(0.,-1.,0.));
#6340=DIRECTION('center_axis',(0.,1.,0.));
#6341=DIRECTION('ref_axis',(1.,0.,0.));
#6342=DIRECTION('center_axis',(0.,1.,0.));
#6343=DIRECTION('ref_axis',(1.,0.,0.));
#6344=DIRECTION('axis',(0.,0.,1.));
#6345=DIRECTION('refdir',(1.,0.,0.));
#6346=DIRECTION('center_axis',(0.866025403784439,0.,-0.5));
#6347=DIRECTION('ref_axis',(0.5,0.,0.866025403784439));
#6348=DIRECTION('',(-0.5,0.,-0.866025403784439));
#6349=DIRECTION('',(0.,-1.,0.));
#6350=DIRECTION('',(0.5,0.,0.866025403784439));
#6351=DIRECTION('',(0.,-1.,0.));
#6352=DIRECTION('center_axis',(1.20185167898973E-16,0.,-1.));
#6353=DIRECTION('ref_axis',(1.,0.,1.20185167898973E-16));
#6354=DIRECTION('',(-1.,0.,-1.20185167898973E-16));
#6355=DIRECTION('',(0.,-1.,0.));
#6356=DIRECTION('',(1.,0.,1.20185167898973E-16));
#6357=DIRECTION('center_axis',(-0.866025403784439,0.,-0.5));
#6358=DIRECTION('ref_axis',(0.5,0.,-0.866025403784439));
#6359=DIRECTION('',(-0.5,0.,0.866025403784439));
#6360=DIRECTION('',(0.,-1.,0.));
#6361=DIRECTION('',(0.5,0.,-0.866025403784439));
#6362=DIRECTION('center_axis',(-0.866025403784439,0.,0.5));
#6363=DIRECTION('ref_axis',(-0.5,0.,-0.866025403784439));
#6364=DIRECTION('',(0.5,0.,0.866025403784439));
#6365=DIRECTION('',(0.,-1.,0.));
#6366=DIRECTION('',(-0.5,0.,-0.866025403784439));
#6367=DIRECTION('center_axis',(-2.40370335797945E-16,0.,1.));
#6368=DIRECTION('ref_axis',(-1.,0.,-2.40370335797945E-16));
#6369=DIRECTION('',(1.,0.,2.40370335797945E-16));
#6370=DIRECTION('',(0.,-1.,0.));
#6371=DIRECTION('',(-1.,0.,-2.40370335797945E-16));
#6372=DIRECTION('center_axis',(0.866025403784439,0.,0.5));
#6373=DIRECTION('ref_axis',(-0.5,0.,0.866025403784439));
#6374=DIRECTION('',(0.5,0.,-0.866025403784439));
#6375=DIRECTION('',(-0.5,0.,0.866025403784439));
#6376=DIRECTION('center_axis',(0.,1.,0.));
#6377=DIRECTION('ref_axis',(1.,0.,0.));
#6378=DIRECTION('center_axis',(0.,-1.,0.));
#6379=DIRECTION('ref_axis',(0.,0.,-1.));
#6380=DIRECTION('center_axis',(0.,1.,0.));
#6381=DIRECTION('ref_axis',(1.,0.,0.));
#6382=DIRECTION('center_axis',(0.,1.,0.));
#6383=DIRECTION('ref_axis',(1.,0.,0.));
#6384=DIRECTION('center_axis',(0.,1.,0.));
#6385=DIRECTION('ref_axis',(0.,0.,1.));
#6386=DIRECTION('center_axis',(0.,-1.,0.));
#6387=DIRECTION('ref_axis',(1.,0.,0.));
#6388=DIRECTION('center_axis',(0.,-1.,0.));
#6389=DIRECTION('ref_axis',(1.,0.,0.));
#6390=DIRECTION('center_axis',(0.,-1.,0.));
#6391=DIRECTION('ref_axis',(1.,0.,0.));
#6392=DIRECTION('',(0.707106781186548,0.707106781186547,8.65956056235493E-17));
#6393=DIRECTION('center_axis',(0.,-1.,0.));
#6394=DIRECTION('ref_axis',(1.,0.,0.));
#6395=DIRECTION('center_axis',(0.,-1.,0.));
#6396=DIRECTION('ref_axis',(1.,0.,0.));
#6397=DIRECTION('',(0.,1.,0.));
#6398=DIRECTION('center_axis',(0.,1.,0.));
#6399=DIRECTION('ref_axis',(1.,0.,0.));
#6400=DIRECTION('center_axis',(0.,-1.,0.));
#6401=DIRECTION('ref_axis',(1.,0.,0.));
#6402=DIRECTION('',(-0.707106781186547,0.707106781186548,-8.65956056235493E-17));
#6403=DIRECTION('center_axis',(0.,-1.,0.));
#6404=DIRECTION('ref_axis',(0.,0.,-1.));
#6405=DIRECTION('center_axis',(0.,-1.,0.));
#6406=DIRECTION('ref_axis',(1.,0.,0.));
#6407=DIRECTION('center_axis',(0.,1.,0.));
#6408=DIRECTION('ref_axis',(1.,0.,0.));
#6409=DIRECTION('center_axis',(0.,1.,0.));
#6410=DIRECTION('ref_axis',(1.,0.,0.));
#6411=DIRECTION('',(-0.447213595499958,0.894427190999916,-5.47678698264203E-17));
#6412=DIRECTION('center_axis',(0.,-1.,0.));
#6413=DIRECTION('ref_axis',(1.,0.,0.));
#6414=DIRECTION('',(0.,1.,0.));
#6415=DIRECTION('axis',(0.,0.,1.));
#6416=DIRECTION('refdir',(1.,0.,0.));
#6417=DIRECTION('center_axis',(1.,0.,0.));
#6418=DIRECTION('ref_axis',(0.,0.,-1.));
#6419=DIRECTION('center_axis',(1.,0.,0.));
#6420=DIRECTION('ref_axis',(0.,0.,-1.));
#6421=DIRECTION('',(1.,0.,0.));
#6422=DIRECTION('center_axis',(-1.,0.,0.));
#6423=DIRECTION('ref_axis',(0.,0.,-1.));
#6424=DIRECTION('center_axis',(1.,0.,0.));
#6425=DIRECTION('ref_axis',(0.,0.,-1.));
#6426=DIRECTION('center_axis',(1.,0.,0.));
#6427=DIRECTION('ref_axis',(0.,0.,-1.));
#6428=DIRECTION('',(1.,0.,0.));
#6429=DIRECTION('center_axis',(-1.,0.,0.));
#6430=DIRECTION('ref_axis',(0.,0.,-1.));
#6431=DIRECTION('center_axis',(1.,0.,0.));
#6432=DIRECTION('ref_axis',(0.,0.,-1.));
#6433=DIRECTION('center_axis',(1.,0.,0.));
#6434=DIRECTION('ref_axis',(0.,0.,-1.));
#6435=DIRECTION('',(1.,0.,0.));
#6436=DIRECTION('center_axis',(-1.,0.,0.));
#6437=DIRECTION('ref_axis',(0.,0.,-1.));
#6438=DIRECTION('center_axis',(1.,0.,0.));
#6439=DIRECTION('ref_axis',(0.,0.,-1.));
#6440=DIRECTION('center_axis',(1.,0.,0.));
#6441=DIRECTION('ref_axis',(0.,0.,-1.));
#6442=DIRECTION('',(1.,0.,0.));
#6443=DIRECTION('center_axis',(-1.,0.,0.));
#6444=DIRECTION('ref_axis',(0.,0.,-1.));
#6445=DIRECTION('center_axis',(1.,0.,0.));
#6446=DIRECTION('ref_axis',(0.,0.,-1.));
#6447=DIRECTION('center_axis',(1.,0.,0.));
#6448=DIRECTION('ref_axis',(0.,0.,-1.));
#6449=DIRECTION('',(1.,0.,0.));
#6450=DIRECTION('center_axis',(-1.,0.,0.));
#6451=DIRECTION('ref_axis',(0.,0.,-1.));
#6452=DIRECTION('center_axis',(1.,0.,0.));
#6453=DIRECTION('ref_axis',(0.,0.,-1.));
#6454=DIRECTION('center_axis',(1.,0.,0.));
#6455=DIRECTION('ref_axis',(0.,0.,-1.));
#6456=DIRECTION('',(1.,0.,0.));
#6457=DIRECTION('center_axis',(-1.,0.,0.));
#6458=DIRECTION('ref_axis',(0.,0.,-1.));
#6459=DIRECTION('center_axis',(1.,0.,0.));
#6460=DIRECTION('ref_axis',(0.,0.,-1.));
#6461=DIRECTION('center_axis',(1.,0.,0.));
#6462=DIRECTION('ref_axis',(0.,0.,-1.));
#6463=DIRECTION('',(1.,0.,0.));
#6464=DIRECTION('center_axis',(-1.,0.,0.));
#6465=DIRECTION('ref_axis',(0.,0.,-1.));
#6466=DIRECTION('center_axis',(1.,0.,0.));
#6467=DIRECTION('ref_axis',(0.,0.,-1.));
#6468=DIRECTION('center_axis',(1.,0.,0.));
#6469=DIRECTION('ref_axis',(0.,0.,-1.));
#6470=DIRECTION('',(1.,0.,0.));
#6471=DIRECTION('center_axis',(-1.,0.,0.));
#6472=DIRECTION('ref_axis',(0.,0.,-1.));
#6473=DIRECTION('center_axis',(1.,0.,0.));
#6474=DIRECTION('ref_axis',(0.,0.,-1.));
#6475=DIRECTION('center_axis',(1.,0.,0.));
#6476=DIRECTION('ref_axis',(0.,0.,-1.));
#6477=DIRECTION('',(1.,0.,0.));
#6478=DIRECTION('center_axis',(-1.,0.,0.));
#6479=DIRECTION('ref_axis',(0.,0.,-1.));
#6480=DIRECTION('center_axis',(1.,0.,0.));
#6481=DIRECTION('ref_axis',(0.,0.,-1.));
#6482=DIRECTION('center_axis',(1.,0.,0.));
#6483=DIRECTION('ref_axis',(0.,0.,-1.));
#6484=DIRECTION('',(1.,0.,0.));
#6485=DIRECTION('center_axis',(-1.,0.,0.));
#6486=DIRECTION('ref_axis',(0.,0.,-1.));
#6487=DIRECTION('center_axis',(1.,0.,0.));
#6488=DIRECTION('ref_axis',(0.,0.,-1.));
#6489=DIRECTION('center_axis',(1.,0.,0.));
#6490=DIRECTION('ref_axis',(0.,0.,-1.));
#6491=DIRECTION('',(1.,0.,0.));
#6492=DIRECTION('center_axis',(-1.,0.,0.));
#6493=DIRECTION('ref_axis',(0.,0.,-1.));
#6494=DIRECTION('center_axis',(1.,0.,0.));
#6495=DIRECTION('ref_axis',(0.,0.,-1.));
#6496=DIRECTION('center_axis',(1.,0.,0.));
#6497=DIRECTION('ref_axis',(0.,0.,-1.));
#6498=DIRECTION('',(1.,0.,0.));
#6499=DIRECTION('center_axis',(-1.,0.,0.));
#6500=DIRECTION('ref_axis',(0.,0.,-1.));
#6501=DIRECTION('center_axis',(1.,0.,0.));
#6502=DIRECTION('ref_axis',(0.,0.,-1.));
#6503=DIRECTION('center_axis',(1.,0.,0.));
#6504=DIRECTION('ref_axis',(0.,0.,-1.));
#6505=DIRECTION('',(1.,0.,0.));
#6506=DIRECTION('center_axis',(-1.,0.,0.));
#6507=DIRECTION('ref_axis',(0.,0.,-1.));
#6508=DIRECTION('center_axis',(1.,0.,0.));
#6509=DIRECTION('ref_axis',(0.,0.,-1.));
#6510=DIRECTION('center_axis',(1.,0.,0.));
#6511=DIRECTION('ref_axis',(0.,0.,-1.));
#6512=DIRECTION('',(1.,0.,0.));
#6513=DIRECTION('center_axis',(-1.,0.,0.));
#6514=DIRECTION('ref_axis',(0.,0.,-1.));
#6515=DIRECTION('center_axis',(1.,0.,0.));
#6516=DIRECTION('ref_axis',(0.,0.,-1.));
#6517=DIRECTION('center_axis',(1.,0.,0.));
#6518=DIRECTION('ref_axis',(0.,0.,-1.));
#6519=DIRECTION('',(1.,0.,0.));
#6520=DIRECTION('center_axis',(-1.,0.,0.));
#6521=DIRECTION('ref_axis',(0.,0.,-1.));
#6522=DIRECTION('center_axis',(1.,0.,0.));
#6523=DIRECTION('ref_axis',(0.,0.,-1.));
#6524=DIRECTION('center_axis',(1.,0.,0.));
#6525=DIRECTION('ref_axis',(0.,0.,-1.));
#6526=DIRECTION('',(1.,0.,0.));
#6527=DIRECTION('center_axis',(-1.,0.,0.));
#6528=DIRECTION('ref_axis',(0.,0.,-1.));
#6529=DIRECTION('center_axis',(1.,0.,0.));
#6530=DIRECTION('ref_axis',(0.,0.,-1.));
#6531=DIRECTION('center_axis',(1.,0.,0.));
#6532=DIRECTION('ref_axis',(0.,0.,-1.));
#6533=DIRECTION('',(1.,0.,0.));
#6534=DIRECTION('center_axis',(-1.,0.,0.));
#6535=DIRECTION('ref_axis',(0.,0.,-1.));
#6536=DIRECTION('center_axis',(1.,0.,0.));
#6537=DIRECTION('ref_axis',(0.,0.,-1.));
#6538=DIRECTION('center_axis',(1.,0.,0.));
#6539=DIRECTION('ref_axis',(0.,0.,-1.));
#6540=DIRECTION('',(1.,0.,0.));
#6541=DIRECTION('center_axis',(-1.,0.,0.));
#6542=DIRECTION('ref_axis',(0.,0.,-1.));
#6543=DIRECTION('center_axis',(1.,0.,0.));
#6544=DIRECTION('ref_axis',(0.,0.,-1.));
#6545=DIRECTION('center_axis',(1.,0.,0.));
#6546=DIRECTION('ref_axis',(0.,0.,-1.));
#6547=DIRECTION('',(1.,0.,0.));
#6548=DIRECTION('center_axis',(-1.,0.,0.));
#6549=DIRECTION('ref_axis',(0.,0.,-1.));
#6550=DIRECTION('center_axis',(1.,0.,0.));
#6551=DIRECTION('ref_axis',(0.,0.,-1.));
#6552=DIRECTION('center_axis',(1.,0.,0.));
#6553=DIRECTION('ref_axis',(0.,0.,-1.));
#6554=DIRECTION('',(1.,0.,0.));
#6555=DIRECTION('center_axis',(-1.,0.,0.));
#6556=DIRECTION('ref_axis',(0.,0.,-1.));
#6557=DIRECTION('center_axis',(1.,0.,0.));
#6558=DIRECTION('ref_axis',(0.,0.,-1.));
#6559=DIRECTION('center_axis',(1.,0.,0.));
#6560=DIRECTION('ref_axis',(0.,0.,-1.));
#6561=DIRECTION('',(1.,0.,0.));
#6562=DIRECTION('center_axis',(-1.,0.,0.));
#6563=DIRECTION('ref_axis',(0.,0.,-1.));
#6564=DIRECTION('center_axis',(1.,0.,0.));
#6565=DIRECTION('ref_axis',(0.,0.,-1.));
#6566=DIRECTION('center_axis',(1.,0.,0.));
#6567=DIRECTION('ref_axis',(0.,0.,-1.));
#6568=DIRECTION('',(1.,0.,0.));
#6569=DIRECTION('center_axis',(-1.,0.,0.));
#6570=DIRECTION('ref_axis',(0.,0.,-1.));
#6571=DIRECTION('center_axis',(1.,0.,0.));
#6572=DIRECTION('ref_axis',(0.,0.,-1.));
#6573=DIRECTION('center_axis',(1.,0.,0.));
#6574=DIRECTION('ref_axis',(0.,0.,-1.));
#6575=DIRECTION('',(1.,0.,0.));
#6576=DIRECTION('center_axis',(-1.,0.,0.));
#6577=DIRECTION('ref_axis',(0.,0.,-1.));
#6578=DIRECTION('center_axis',(1.,0.,0.));
#6579=DIRECTION('ref_axis',(0.,0.,-1.));
#6580=DIRECTION('center_axis',(1.,0.,0.));
#6581=DIRECTION('ref_axis',(0.,0.,-1.));
#6582=DIRECTION('',(1.,0.,0.));
#6583=DIRECTION('center_axis',(-1.,0.,0.));
#6584=DIRECTION('ref_axis',(0.,0.,-1.));
#6585=DIRECTION('center_axis',(1.,0.,0.));
#6586=DIRECTION('ref_axis',(0.,0.,-1.));
#6587=DIRECTION('center_axis',(1.,0.,0.));
#6588=DIRECTION('ref_axis',(0.,0.,-1.));
#6589=DIRECTION('',(1.,0.,0.));
#6590=DIRECTION('center_axis',(-1.,0.,0.));
#6591=DIRECTION('ref_axis',(0.,0.,-1.));
#6592=DIRECTION('center_axis',(1.,0.,0.));
#6593=DIRECTION('ref_axis',(0.,0.,-1.));
#6594=DIRECTION('center_axis',(1.,0.,0.));
#6595=DIRECTION('ref_axis',(0.,0.,-1.));
#6596=DIRECTION('',(1.,0.,0.));
#6597=DIRECTION('center_axis',(-1.,0.,0.));
#6598=DIRECTION('ref_axis',(0.,0.,-1.));
#6599=DIRECTION('center_axis',(1.,0.,0.));
#6600=DIRECTION('ref_axis',(0.,0.,-1.));
#6601=DIRECTION('center_axis',(1.,0.,0.));
#6602=DIRECTION('ref_axis',(0.,0.,-1.));
#6603=DIRECTION('',(1.,0.,0.));
#6604=DIRECTION('center_axis',(-1.,0.,0.));
#6605=DIRECTION('ref_axis',(0.,0.,-1.));
#6606=DIRECTION('center_axis',(1.,0.,0.));
#6607=DIRECTION('ref_axis',(0.,0.,-1.));
#6608=DIRECTION('center_axis',(1.,0.,0.));
#6609=DIRECTION('ref_axis',(0.,0.,-1.));
#6610=DIRECTION('',(1.,0.,0.));
#6611=DIRECTION('center_axis',(-1.,0.,0.));
#6612=DIRECTION('ref_axis',(0.,0.,-1.));
#6613=DIRECTION('center_axis',(0.,1.,0.));
#6614=DIRECTION('ref_axis',(-1.,0.,0.));
#6615=DIRECTION('',(-1.,0.,0.));
#6616=DIRECTION('',(0.,0.,1.));
#6617=DIRECTION('',(-1.,0.,0.));
#6618=DIRECTION('',(0.,0.,1.));
#6619=DIRECTION('center_axis',(1.,0.,0.));
#6620=DIRECTION('ref_axis',(0.,1.,0.));
#6621=DIRECTION('',(0.,1.,0.));
#6622=DIRECTION('',(0.,1.,0.));
#6623=DIRECTION('',(0.,0.,1.));
#6624=DIRECTION('center_axis',(0.,-1.,0.));
#6625=DIRECTION('ref_axis',(1.,0.,0.));
#6626=DIRECTION('',(1.,0.,0.));
#6627=DIRECTION('',(1.,0.,0.));
#6628=DIRECTION('',(0.,0.,1.));
#6629=DIRECTION('center_axis',(-1.,0.,0.));
#6630=DIRECTION('ref_axis',(0.,-1.,0.));
#6631=DIRECTION('',(0.,-1.,0.));
#6632=DIRECTION('',(0.,-1.,0.));
#6633=DIRECTION('center_axis',(0.,0.,1.));
#6634=DIRECTION('ref_axis',(1.,0.,0.));
#6635=DIRECTION('center_axis',(0.,0.,1.));
#6636=DIRECTION('ref_axis',(1.,0.,0.));
#6637=DIRECTION('axis',(0.,0.,1.));
#6638=DIRECTION('refdir',(1.,0.,0.));
#6639=DIRECTION('center_axis',(1.,0.,0.));
#6640=DIRECTION('ref_axis',(0.,0.,-1.));
#6641=DIRECTION('center_axis',(1.,0.,0.));
#6642=DIRECTION('ref_axis',(0.,0.,-1.));
#6643=DIRECTION('',(1.,0.,0.));
#6644=DIRECTION('center_axis',(-1.,0.,0.));
#6645=DIRECTION('ref_axis',(0.,0.,-1.));
#6646=DIRECTION('center_axis',(1.,0.,0.));
#6647=DIRECTION('ref_axis',(0.,0.,-1.));
#6648=DIRECTION('center_axis',(1.,0.,0.));
#6649=DIRECTION('ref_axis',(0.,0.,-1.));
#6650=DIRECTION('',(1.,0.,0.));
#6651=DIRECTION('center_axis',(-1.,0.,0.));
#6652=DIRECTION('ref_axis',(0.,0.,-1.));
#6653=DIRECTION('center_axis',(0.,1.,0.));
#6654=DIRECTION('ref_axis',(-1.,0.,0.));
#6655=DIRECTION('',(-1.,0.,0.));
#6656=DIRECTION('',(0.,0.,1.));
#6657=DIRECTION('',(-1.,0.,0.));
#6658=DIRECTION('',(0.,0.,1.));
#6659=DIRECTION('center_axis',(1.,0.,0.));
#6660=DIRECTION('ref_axis',(0.,1.,0.));
#6661=DIRECTION('',(0.,1.,0.));
#6662=DIRECTION('',(0.,1.,0.));
#6663=DIRECTION('',(0.,0.,1.));
#6664=DIRECTION('center_axis',(0.,-1.,0.));
#6665=DIRECTION('ref_axis',(1.,0.,0.));
#6666=DIRECTION('',(1.,0.,0.));
#6667=DIRECTION('',(1.,0.,0.));
#6668=DIRECTION('',(0.,0.,1.));
#6669=DIRECTION('center_axis',(-1.,0.,0.));
#6670=DIRECTION('ref_axis',(0.,-1.,0.));
#6671=DIRECTION('',(0.,-1.,0.));
#6672=DIRECTION('',(0.,-1.,0.));
#6673=DIRECTION('center_axis',(0.,0.,1.));
#6674=DIRECTION('ref_axis',(1.,0.,0.));
#6675=DIRECTION('center_axis',(0.,0.,1.));
#6676=DIRECTION('ref_axis',(1.,0.,0.));
#6677=DIRECTION('axis',(0.,0.,1.));
#6678=DIRECTION('refdir',(1.,0.,0.));
#6679=DIRECTION('center_axis',(0.,-1.,0.));
#6680=DIRECTION('ref_axis',(1.,0.,0.));
#6681=DIRECTION('center_axis',(0.,1.,0.));
#6682=DIRECTION('ref_axis',(1.,0.,0.));
#6683=DIRECTION('',(0.,1.,0.));
#6684=DIRECTION('center_axis',(0.,-1.,0.));
#6685=DIRECTION('ref_axis',(1.,0.,0.));
#6686=DIRECTION('center_axis',(0.,1.,0.));
#6687=DIRECTION('ref_axis',(1.,0.,0.));
#6688=DIRECTION('center_axis',(0.,-1.,0.));
#6689=DIRECTION('ref_axis',(1.,0.,0.));
#6690=DIRECTION('',(-0.707106781186547,0.707106781186548,-8.65956056235493E-17));
#6691=DIRECTION('center_axis',(0.,-1.,0.));
#6692=DIRECTION('ref_axis',(0.,0.,-1.));
#6693=DIRECTION('center_axis',(0.,-1.,0.));
#6694=DIRECTION('ref_axis',(1.,0.,0.));
#6695=DIRECTION('center_axis',(0.,1.,0.));
#6696=DIRECTION('ref_axis',(1.,0.,0.));
#6697=DIRECTION('',(-0.866025403784439,-0.5,-1.06057523872491E-16));
#6698=DIRECTION('center_axis',(1.92296268638356E-16,0.,-1.));
#6699=DIRECTION('ref_axis',(-1.,0.,-1.92296268638356E-16));
#6700=DIRECTION('',(0.,1.,0.));
#6701=DIRECTION('',(-1.,0.,-1.92296268638356E-16));
#6702=DIRECTION('',(0.,1.,0.));
#6703=DIRECTION('center_axis',(0.866025403784439,0.,-0.5));
#6704=DIRECTION('ref_axis',(-0.5,0.,-0.866025403784439));
#6705=DIRECTION('',(0.,1.,0.));
#6706=DIRECTION('',(-0.5,0.,-0.866025403784439));
#6707=DIRECTION('center_axis',(0.866025403784439,0.,0.5));
#6708=DIRECTION('ref_axis',(0.5,0.,-0.866025403784439));
#6709=DIRECTION('',(0.,1.,0.));
#6710=DIRECTION('',(0.5,0.,-0.866025403784439));
#6711=DIRECTION('center_axis',(-1.92296268638356E-16,0.,1.));
#6712=DIRECTION('ref_axis',(1.,0.,1.92296268638356E-16));
#6713=DIRECTION('',(0.,1.,0.));
#6714=DIRECTION('',(1.,0.,1.92296268638356E-16));
#6715=DIRECTION('center_axis',(-0.866025403784439,0.,0.5));
#6716=DIRECTION('ref_axis',(0.5,0.,0.866025403784439));
#6717=DIRECTION('',(0.,1.,0.));
#6718=DIRECTION('',(0.5,0.,0.866025403784439));
#6719=DIRECTION('center_axis',(-0.866025403784439,0.,-0.5));
#6720=DIRECTION('ref_axis',(-0.5,0.,0.866025403784439));
#6721=DIRECTION('',(-0.5,0.,0.866025403784438));
#6722=DIRECTION('center_axis',(0.,1.,0.));
#6723=DIRECTION('ref_axis',(0.,0.,1.));
#6724=DIRECTION('center_axis',(0.,1.,0.));
#6725=DIRECTION('ref_axis',(1.,0.,0.));
#6726=DIRECTION('axis',(0.,0.,1.));
#6727=DIRECTION('refdir',(1.,0.,0.));
#6728=DIRECTION('center_axis',(0.,1.,0.));
#6729=DIRECTION('ref_axis',(1.,0.,0.));
#6730=DIRECTION('',(0.866025403784439,-0.5,1.06057523872491E-16));
#6731=DIRECTION('center_axis',(0.,-1.,0.));
#6732=DIRECTION('ref_axis',(1.,0.,0.));
#6733=DIRECTION('center_axis',(0.,-1.,0.));
#6734=DIRECTION('ref_axis',(1.,0.,0.));
#6735=DIRECTION('center_axis',(0.,1.,0.));
#6736=DIRECTION('ref_axis',(1.,0.,0.));
#6737=DIRECTION('',(-0.866025403784439,-0.5,-1.06057523872491E-16));
#6738=DIRECTION('center_axis',(1.92296268638356E-16,0.,-1.));
#6739=DIRECTION('ref_axis',(-1.,0.,-1.92296268638356E-16));
#6740=DIRECTION('',(0.,1.,0.));
#6741=DIRECTION('',(0.,1.,0.));
#6742=DIRECTION('center_axis',(-0.866025403784439,0.,-0.5));
#6743=DIRECTION('ref_axis',(-0.5,0.,0.866025403784439));
#6744=DIRECTION('',(0.,1.,0.));
#6745=DIRECTION('center_axis',(-0.866025403784439,0.,0.5));
#6746=DIRECTION('ref_axis',(0.5,0.,0.866025403784439));
#6747=DIRECTION('',(0.,1.,0.));
#6748=DIRECTION('center_axis',(0.,1.,0.));
#6749=DIRECTION('ref_axis',(1.,0.,0.));
#6750=DIRECTION('center_axis',(0.,1.,0.));
#6751=DIRECTION('ref_axis',(1.,0.,0.));
#6752=DIRECTION('',(0.,-1.,0.));
#6753=DIRECTION('center_axis',(0.,1.,0.));
#6754=DIRECTION('ref_axis',(1.,0.,0.));
#6755=DIRECTION('center_axis',(-1.92296268638356E-16,0.,1.));
#6756=DIRECTION('ref_axis',(1.,0.,1.92296268638356E-16));
#6757=DIRECTION('',(0.,1.,0.));
#6758=DIRECTION('center_axis',(0.866025403784439,0.,-0.5));
#6759=DIRECTION('ref_axis',(-0.5,0.,-0.866025403784439));
#6760=DIRECTION('',(0.,1.,0.));
#6761=DIRECTION('center_axis',(0.866025403784439,0.,0.5));
#6762=DIRECTION('ref_axis',(0.5,0.,-0.866025403784439));
#6763=DIRECTION('center_axis',(0.,1.,0.));
#6764=DIRECTION('ref_axis',(1.,0.,0.));
#6765=DIRECTION('center_axis',(0.,1.,0.));
#6766=DIRECTION('ref_axis',(1.,0.,0.));
#6767=DIRECTION('axis',(0.,0.,1.));
#6768=DIRECTION('refdir',(1.,0.,0.));
#6769=DIRECTION('center_axis',(1.,0.,0.));
#6770=DIRECTION('ref_axis',(0.,0.,-1.));
#6771=DIRECTION('center_axis',(1.,0.,0.));
#6772=DIRECTION('ref_axis',(0.,0.,-1.));
#6773=DIRECTION('',(-1.,0.,0.));
#6774=DIRECTION('center_axis',(-1.,0.,0.));
#6775=DIRECTION('ref_axis',(0.,0.,-1.));
#6776=DIRECTION('center_axis',(1.,0.,0.));
#6777=DIRECTION('ref_axis',(0.,0.,-1.));
#6778=DIRECTION('center_axis',(1.,0.,0.));
#6779=DIRECTION('ref_axis',(0.,0.,-1.));
#6780=DIRECTION('center_axis',(1.,0.,0.));
#6781=DIRECTION('ref_axis',(0.,0.,-1.));
#6782=DIRECTION('',(-1.,0.,0.));
#6783=DIRECTION('center_axis',(1.,0.,0.));
#6784=DIRECTION('ref_axis',(0.,0.,-1.));
#6785=DIRECTION('center_axis',(1.,0.,0.));
#6786=DIRECTION('ref_axis',(0.,0.,-1.));
#6787=DIRECTION('center_axis',(1.,0.,0.));
#6788=DIRECTION('ref_axis',(0.,0.,-1.));
#6789=DIRECTION('axis',(0.,0.,1.));
#6790=DIRECTION('refdir',(1.,0.,0.));
#6791=DIRECTION('center_axis',(6.12323399573677E-17,0.,1.));
#6792=DIRECTION('ref_axis',(1.,0.,0.));
#6793=DIRECTION('center_axis',(0.,-1.,0.));
#6794=DIRECTION('ref_axis',(1.,0.,0.));
#6795=DIRECTION('center_axis',(0.,-1.,0.));
#6796=DIRECTION('ref_axis',(1.,0.,0.));
#6797=DIRECTION('center_axis',(0.,-1.,0.));
#6798=DIRECTION('ref_axis',(1.,0.,0.));
#6799=DIRECTION('',(0.,1.,0.));
#6800=DIRECTION('center_axis',(0.,1.,0.));
#6801=DIRECTION('ref_axis',(1.,0.,0.));
#6802=DIRECTION('center_axis',(0.,-1.,0.));
#6803=DIRECTION('ref_axis',(1.,0.,0.));
#6804=DIRECTION('',(-0.707106781186547,0.707106781186548,-8.65956056235493E-17));
#6805=DIRECTION('center_axis',(0.,-1.,0.));
#6806=DIRECTION('ref_axis',(0.,0.,-1.));
#6807=DIRECTION('axis',(0.,0.,1.));
#6808=DIRECTION('refdir',(1.,0.,0.));
#6809=DIRECTION('center_axis',(0.,1.,0.));
#6810=DIRECTION('ref_axis',(0.,0.,1.));
#6811=DIRECTION('center_axis',(0.,1.,0.));
#6812=DIRECTION('ref_axis',(1.,0.,0.));
#6813=DIRECTION('',(0.,0.,1.));
#6814=DIRECTION('center_axis',(1.,0.,0.));
#6815=DIRECTION('ref_axis',(0.,0.,-1.));
#6816=DIRECTION('',(0.,1.,0.));
#6817=DIRECTION('',(0.,0.,1.));
#6818=DIRECTION('',(0.,-1.,0.));
#6819=DIRECTION('center_axis',(0.,-1.,0.));
#6820=DIRECTION('ref_axis',(1.,0.,0.));
#6821=DIRECTION('center_axis',(0.,-1.,0.));
#6822=DIRECTION('ref_axis',(1.,0.,0.));
#6823=DIRECTION('',(0.,1.,0.));
#6824=DIRECTION('center_axis',(0.,1.,0.));
#6825=DIRECTION('ref_axis',(1.,0.,0.));
#6826=DIRECTION('',(0.,1.,0.));
#6827=DIRECTION('center_axis',(0.,-1.,0.));
#6828=DIRECTION('ref_axis',(1.,0.,0.));
#6829=DIRECTION('center_axis',(0.,1.,0.));
#6830=DIRECTION('ref_axis',(1.,0.,0.));
#6831=DIRECTION('',(0.,-1.,0.));
#6832=DIRECTION('center_axis',(0.,-1.,0.));
#6833=DIRECTION('ref_axis',(1.,0.,0.));
#6834=DIRECTION('center_axis',(0.,1.,0.));
#6835=DIRECTION('ref_axis',(1.,0.,0.));
#6836=DIRECTION('center_axis',(0.,-1.,0.));
#6837=DIRECTION('ref_axis',(1.,0.,0.));
#6838=DIRECTION('center_axis',(1.,0.,0.));
#6839=DIRECTION('ref_axis',(0.,0.,-1.));
#6840=DIRECTION('',(0.,0.,1.));
#6841=DIRECTION('',(0.,0.,-1.));
#6842=DIRECTION('center_axis',(0.,1.,0.));
#6843=DIRECTION('ref_axis',(0.,0.,1.));
#6844=DIRECTION('center_axis',(0.,-1.,0.));
#6845=DIRECTION('ref_axis',(0.,0.,-1.));
#6846=DIRECTION('center_axis',(0.,-1.,0.));
#6847=DIRECTION('ref_axis',(1.,0.,0.));
#6848=DIRECTION('center_axis',(6.12323399573677E-17,0.,1.));
#6849=DIRECTION('ref_axis',(1.,0.,0.));
#6850=DIRECTION('center_axis',(0.,1.,0.));
#6851=DIRECTION('ref_axis',(1.,0.,0.));
#6852=DIRECTION('axis',(0.,0.,1.));
#6853=DIRECTION('refdir',(1.,0.,0.));
#6854=DIRECTION('center_axis',(0.866025403784439,0.,-0.5));
#6855=DIRECTION('ref_axis',(0.5,0.,0.866025403784439));
#6856=DIRECTION('',(-0.5,0.,-0.866025403784439));
#6857=DIRECTION('',(0.,-1.,0.));
#6858=DIRECTION('',(0.5,0.,0.866025403784439));
#6859=DIRECTION('',(0.,-1.,0.));
#6860=DIRECTION('center_axis',(1.60246890531964E-16,0.,-1.));
#6861=DIRECTION('ref_axis',(1.,0.,1.60246890531964E-16));
#6862=DIRECTION('',(-1.,0.,-1.60246890531964E-16));
#6863=DIRECTION('',(0.,-1.,0.));
#6864=DIRECTION('',(1.,0.,1.60246890531964E-16));
#6865=DIRECTION('center_axis',(-0.866025403784439,0.,-0.5));
#6866=DIRECTION('ref_axis',(0.5,0.,-0.866025403784439));
#6867=DIRECTION('',(-0.5,0.,0.866025403784439));
#6868=DIRECTION('',(0.,-1.,0.));
#6869=DIRECTION('',(0.5,0.,-0.866025403784439));
#6870=DIRECTION('center_axis',(-0.866025403784439,0.,0.5));
#6871=DIRECTION('ref_axis',(-0.5,0.,-0.866025403784439));
#6872=DIRECTION('',(0.5,0.,0.866025403784439));
#6873=DIRECTION('',(0.,-1.,0.));
#6874=DIRECTION('',(-0.5,0.,-0.866025403784439));
#6875=DIRECTION('center_axis',(-1.60246890531964E-16,0.,1.));
#6876=DIRECTION('ref_axis',(-1.,0.,-1.60246890531964E-16));
#6877=DIRECTION('',(1.,0.,1.60246890531964E-16));
#6878=DIRECTION('',(0.,-1.,0.));
#6879=DIRECTION('',(-1.,0.,-1.60246890531964E-16));
#6880=DIRECTION('center_axis',(0.866025403784439,0.,0.5));
#6881=DIRECTION('ref_axis',(-0.5,0.,0.866025403784439));
#6882=DIRECTION('',(0.5,0.,-0.866025403784439));
#6883=DIRECTION('',(-0.5,0.,0.866025403784439));
#6884=DIRECTION('center_axis',(0.,1.,0.));
#6885=DIRECTION('ref_axis',(1.,0.,0.));
#6886=DIRECTION('center_axis',(0.,-1.,0.));
#6887=DIRECTION('ref_axis',(0.,0.,-1.));
#6888=DIRECTION('center_axis',(0.,1.,0.));
#6889=DIRECTION('ref_axis',(1.,0.,0.));
#6890=DIRECTION('center_axis',(0.,1.,0.));
#6891=DIRECTION('ref_axis',(1.,0.,0.));
#6892=DIRECTION('center_axis',(0.,1.,0.));
#6893=DIRECTION('ref_axis',(0.,0.,1.));
#6894=DIRECTION('center_axis',(0.,-1.,0.));
#6895=DIRECTION('ref_axis',(1.,0.,0.));
#6896=DIRECTION('center_axis',(0.,-1.,0.));
#6897=DIRECTION('ref_axis',(1.,0.,0.));
#6898=DIRECTION('center_axis',(0.,-1.,0.));
#6899=DIRECTION('ref_axis',(1.,0.,0.));
#6900=DIRECTION('',(0.707106781186548,0.707106781186547,8.65956056235493E-17));
#6901=DIRECTION('center_axis',(0.,-1.,0.));
#6902=DIRECTION('ref_axis',(1.,0.,0.));
#6903=DIRECTION('center_axis',(0.,-1.,0.));
#6904=DIRECTION('ref_axis',(1.,0.,0.));
#6905=DIRECTION('',(0.,1.,0.));
#6906=DIRECTION('center_axis',(0.,1.,0.));
#6907=DIRECTION('ref_axis',(1.,0.,0.));
#6908=DIRECTION('center_axis',(0.,-1.,0.));
#6909=DIRECTION('ref_axis',(1.,0.,0.));
#6910=DIRECTION('',(-0.707106781186548,0.707106781186547,-8.65956056235494E-17));
#6911=DIRECTION('center_axis',(0.,-1.,0.));
#6912=DIRECTION('ref_axis',(0.,0.,-1.));
#6913=DIRECTION('center_axis',(0.,-1.,0.));
#6914=DIRECTION('ref_axis',(1.,0.,0.));
#6915=DIRECTION('center_axis',(0.,1.,0.));
#6916=DIRECTION('ref_axis',(1.,0.,0.));
#6917=DIRECTION('center_axis',(0.,1.,0.));
#6918=DIRECTION('ref_axis',(1.,0.,0.));
#6919=DIRECTION('',(-0.447213595499958,0.894427190999916,-5.47678698264203E-17));
#6920=DIRECTION('center_axis',(0.,-1.,0.));
#6921=DIRECTION('ref_axis',(1.,0.,0.));
#6922=DIRECTION('',(0.,1.,0.));
#6923=DIRECTION('axis',(0.,0.,1.));
#6924=DIRECTION('refdir',(1.,0.,0.));
#6925=DIRECTION('axis',(0.,0.,1.));
#6926=DIRECTION('refdir',(1.,0.,0.));
#6927=DIRECTION('center_axis',(0.,1.,0.));
#6928=DIRECTION('ref_axis',(1.,0.,0.));
#6929=DIRECTION('center_axis',(0.,1.,0.));
#6930=DIRECTION('ref_axis',(1.,0.,0.));
#6931=DIRECTION('',(0.,1.,0.));
#6932=DIRECTION('center_axis',(0.,-1.,0.));
#6933=DIRECTION('ref_axis',(1.,0.,0.));
#6934=DIRECTION('center_axis',(0.,1.,0.));
#6935=DIRECTION('ref_axis',(1.,0.,0.));
#6936=DIRECTION('center_axis',(0.,1.,0.));
#6937=DIRECTION('ref_axis',(1.,0.,0.));
#6938=DIRECTION('',(0.,1.,0.));
#6939=DIRECTION('center_axis',(0.,-1.,0.));
#6940=DIRECTION('ref_axis',(1.,0.,0.));
#6941=DIRECTION('center_axis',(0.,1.,0.));
#6942=DIRECTION('ref_axis',(0.0871557427476581,0.,0.996194698091746));
#6943=DIRECTION('',(0.,-1.,0.));
#6944=DIRECTION('center_axis',(0.,1.,0.));
#6945=DIRECTION('ref_axis',(1.,0.,0.));
#6946=DIRECTION('',(0.,1.,0.));
#6947=DIRECTION('center_axis',(0.,1.,0.));
#6948=DIRECTION('ref_axis',(1.,0.,0.));
#6949=DIRECTION('center_axis',(0.,1.,0.));
#6950=DIRECTION('ref_axis',(1.,0.,0.));
#6951=DIRECTION('',(0.0871557427476582,0.,0.996194698091746));
#6952=DIRECTION('center_axis',(0.,-1.,0.));
#6953=DIRECTION('ref_axis',(1.,0.,0.));
#6954=DIRECTION('',(-0.0871557427476581,0.,-0.996194698091746));
#6955=DIRECTION('center_axis',(-0.996194698091746,0.,0.0871557427476582));
#6956=DIRECTION('ref_axis',(0.0871557427476582,0.,0.996194698091746));
#6957=DIRECTION('',(0.0871557427476582,0.,0.996194698091746));
#6958=DIRECTION('',(0.,1.,0.));
#6959=DIRECTION('center_axis',(0.,1.,0.));
#6960=DIRECTION('ref_axis',(0.,0.,1.));
#6961=DIRECTION('',(-0.0871557427476581,0.,-0.996194698091746));
#6962=DIRECTION('center_axis',(0.,1.,0.));
#6963=DIRECTION('ref_axis',(1.,0.,0.));
#6964=DIRECTION('center_axis',(0.996194698091746,0.,-0.0871557427476581));
#6965=DIRECTION('ref_axis',(-0.0871557427476581,0.,-0.996194698091746));
#6966=DIRECTION('',(0.,-1.,0.));
#6967=DIRECTION('center_axis',(0.,1.,0.));
#6968=DIRECTION('ref_axis',(1.,0.,0.));
#6969=DIRECTION('center_axis',(0.,1.,0.));
#6970=DIRECTION('ref_axis',(1.,0.,0.));
#6971=DIRECTION('',(0.,1.,0.));
#6972=DIRECTION('center_axis',(0.,-1.,0.));
#6973=DIRECTION('ref_axis',(1.,0.,0.));
#6974=DIRECTION('center_axis',(0.,1.,0.));
#6975=DIRECTION('ref_axis',(1.,0.,0.));
#6976=DIRECTION('center_axis',(0.,1.,0.));
#6977=DIRECTION('ref_axis',(1.,0.,0.));
#6978=DIRECTION('',(0.,1.,0.));
#6979=DIRECTION('center_axis',(0.,-1.,0.));
#6980=DIRECTION('ref_axis',(1.,0.,0.));
#6981=DIRECTION('center_axis',(0.996194698091746,0.,-0.0871557427476583));
#6982=DIRECTION('ref_axis',(-0.0871557427476583,0.,-0.996194698091746));
#6983=DIRECTION('',(0.0871557427476583,0.,0.996194698091746));
#6984=DIRECTION('',(0.,1.,0.));
#6985=DIRECTION('',(-0.0871557427476583,0.,-0.996194698091746));
#6986=DIRECTION('',(0.,1.,0.));
#6987=DIRECTION('center_axis',(0.,1.,0.));
#6988=DIRECTION('ref_axis',(0.,0.,1.));
#6989=DIRECTION('',(0.996194698091746,0.,-0.0871557427476581));
#6990=DIRECTION('',(-0.087155742747658,0.,-0.996194698091746));
#6991=DIRECTION('',(-0.996194698091746,0.,0.0871557427476581));
#6992=DIRECTION('',(0.0871557427476582,0.,0.996194698091746));
#6993=DIRECTION('center_axis',(0.996194698091746,0.,-0.087155742747658));
#6994=DIRECTION('ref_axis',(-0.087155742747658,0.,-0.996194698091746));
#6995=DIRECTION('',(0.087155742747658,0.,0.996194698091746));
#6996=DIRECTION('',(0.,1.,0.));
#6997=DIRECTION('',(0.,1.,0.));
#6998=DIRECTION('center_axis',(0.,1.,0.));
#6999=DIRECTION('ref_axis',(1.,0.,0.));
#7000=DIRECTION('',(0.996194698091746,0.,-0.0871557427476581));
#7001=DIRECTION('',(-0.996194698091746,0.,0.0871557427476581));
#7002=DIRECTION('center_axis',(0.,1.,0.));
#7003=DIRECTION('ref_axis',(1.,0.,0.));
#7004=DIRECTION('',(0.0871557427476582,0.,0.996194698091746));
#7005=DIRECTION('',(0.996194698091746,0.,-0.0871557427476581));
#7006=DIRECTION('center_axis',(0.,-1.,0.));
#7007=DIRECTION('ref_axis',(1.,0.,0.));
#7008=DIRECTION('',(-0.996194698091746,0.,0.087155742747658));
#7009=DIRECTION('center_axis',(0.0871557427476581,0.,0.996194698091746));
#7010=DIRECTION('ref_axis',(0.996194698091746,0.,-0.0871557427476581));
#7011=DIRECTION('',(0.,1.,0.));
#7012=DIRECTION('',(0.996194698091746,0.,-0.0871557427476581));
#7013=DIRECTION('',(0.,1.,0.));
#7014=DIRECTION('center_axis',(0.,1.,0.));
#7015=DIRECTION('ref_axis',(0.,0.,1.));
#7016=DIRECTION('',(-0.0871557427476582,0.,-0.996194698091746));
#7017=DIRECTION('',(-0.996194698091746,0.,0.087155742747658));
#7018=DIRECTION('center_axis',(0.,1.,0.));
#7019=DIRECTION('ref_axis',(1.,0.,0.));
#7020=DIRECTION('center_axis',(-0.087155742747658,0.,-0.996194698091746));
#7021=DIRECTION('ref_axis',(-0.996194698091746,0.,0.087155742747658));
#7022=DIRECTION('',(0.,-1.,0.));
#7023=DIRECTION('',(0.,-1.,0.));
#7024=DIRECTION('center_axis',(0.,1.,0.));
#7025=DIRECTION('ref_axis',(1.,0.,0.));
#7026=DIRECTION('center_axis',(0.,1.,0.));
#7027=DIRECTION('ref_axis',(1.,0.,0.));
#7028=DIRECTION('',(0.,-1.,0.));
#7029=DIRECTION('center_axis',(0.,1.,0.));
#7030=DIRECTION('ref_axis',(1.,0.,0.));
#7031=DIRECTION('center_axis',(0.,1.,0.));
#7032=DIRECTION('ref_axis',(1.,0.,0.));
#7033=DIRECTION('center_axis',(0.,1.,0.));
#7034=DIRECTION('ref_axis',(1.,0.,0.));
#7035=DIRECTION('center_axis',(-0.0871557427476581,0.,-0.996194698091746));
#7036=DIRECTION('ref_axis',(-0.996194698091746,0.,0.0871557427476581));
#7037=DIRECTION('',(-0.996194698091746,0.,0.0871557427476581));
#7038=DIRECTION('',(0.,1.,0.));
#7039=DIRECTION('',(0.996194698091746,0.,-0.0871557427476581));
#7040=DIRECTION('',(0.,1.,0.));
#7041=DIRECTION('center_axis',(0.,1.,0.));
#7042=DIRECTION('ref_axis',(0.,0.,1.));
#7043=DIRECTION('',(0.996194698091746,0.,-0.0871557427476581));
#7044=DIRECTION('',(-0.087155742747658,0.,-0.996194698091746));
#7045=DIRECTION('center_axis',(-0.996194698091746,0.,0.0871557427476582));
#7046=DIRECTION('ref_axis',(0.0871557427476582,0.,0.996194698091746));
#7047=DIRECTION('',(-0.0871557427476582,0.,-0.996194698091746));
#7048=DIRECTION('',(0.,1.,0.));
#7049=DIRECTION('center_axis',(0.996194698091746,0.,-0.087155742747658));
#7050=DIRECTION('ref_axis',(-0.087155742747658,0.,-0.996194698091746));
#7051=DIRECTION('',(0.087155742747658,0.,0.996194698091746));
#7052=DIRECTION('',(0.,1.,0.));
#7053=DIRECTION('center_axis',(0.0871557427476581,0.,0.996194698091746));
#7054=DIRECTION('ref_axis',(0.996194698091746,0.,-0.0871557427476581));
#7055=DIRECTION('',(-0.996194698091746,0.,0.0871557427476581));
#7056=DIRECTION('center_axis',(0.,1.,0.));
#7057=DIRECTION('ref_axis',(1.,0.,0.));
#7058=DIRECTION('axis',(0.,0.,1.));
#7059=DIRECTION('refdir',(1.,0.,0.));
#7060=DIRECTION('center_axis',(0.,1.,0.));
#7061=DIRECTION('ref_axis',(1.,0.,0.));
#7062=DIRECTION('center_axis',(0.,1.,0.));
#7063=DIRECTION('ref_axis',(1.,0.,0.));
#7064=DIRECTION('',(0.,1.,0.));
#7065=DIRECTION('center_axis',(0.,-1.,0.));
#7066=DIRECTION('ref_axis',(1.,0.,0.));
#7067=DIRECTION('center_axis',(0.,1.,0.));
#7068=DIRECTION('ref_axis',(1.,0.,0.));
#7069=DIRECTION('center_axis',(0.,1.,0.));
#7070=DIRECTION('ref_axis',(1.,0.,0.));
#7071=DIRECTION('center_axis',(0.,1.,0.));
#7072=DIRECTION('ref_axis',(1.,0.,0.));
#7073=DIRECTION('',(0.,-1.,0.));
#7074=DIRECTION('center_axis',(0.,1.,0.));
#7075=DIRECTION('ref_axis',(1.,0.,0.));
#7076=DIRECTION('center_axis',(0.,1.,0.));
#7077=DIRECTION('ref_axis',(1.,0.,0.));
#7078=DIRECTION('center_axis',(0.,1.,0.));
#7079=DIRECTION('ref_axis',(1.,0.,0.));
#7080=DIRECTION('axis',(0.,0.,1.));
#7081=DIRECTION('refdir',(1.,0.,0.));
#7082=DIRECTION('center_axis',(0.866025403784439,0.,-0.5));
#7083=DIRECTION('ref_axis',(0.5,0.,0.866025403784439));
#7084=DIRECTION('',(-0.5,0.,-0.866025403784439));
#7085=DIRECTION('',(0.,-1.,0.));
#7086=DIRECTION('',(0.5,0.,0.866025403784439));
#7087=DIRECTION('',(0.,-1.,0.));
#7088=DIRECTION('center_axis',(1.20185167898973E-16,0.,-1.));
#7089=DIRECTION('ref_axis',(1.,0.,1.20185167898973E-16));
#7090=DIRECTION('',(-1.,0.,-1.20185167898973E-16));
#7091=DIRECTION('',(0.,-1.,0.));
#7092=DIRECTION('',(1.,0.,1.20185167898973E-16));
#7093=DIRECTION('center_axis',(-0.866025403784439,0.,-0.5));
#7094=DIRECTION('ref_axis',(0.5,0.,-0.866025403784439));
#7095=DIRECTION('',(-0.5,0.,0.866025403784439));
#7096=DIRECTION('',(0.,-1.,0.));
#7097=DIRECTION('',(0.5,0.,-0.866025403784439));
#7098=DIRECTION('center_axis',(-0.866025403784439,0.,0.5));
#7099=DIRECTION('ref_axis',(-0.5,0.,-0.866025403784439));
#7100=DIRECTION('',(0.5,0.,0.866025403784439));
#7101=DIRECTION('',(0.,-1.,0.));
#7102=DIRECTION('',(-0.5,0.,-0.866025403784439));
#7103=DIRECTION('center_axis',(-2.40370335797945E-16,0.,1.));
#7104=DIRECTION('ref_axis',(-1.,0.,-2.40370335797945E-16));
#7105=DIRECTION('',(1.,0.,2.40370335797945E-16));
#7106=DIRECTION('',(0.,-1.,0.));
#7107=DIRECTION('',(-1.,0.,-2.40370335797945E-16));
#7108=DIRECTION('center_axis',(0.866025403784439,0.,0.5));
#7109=DIRECTION('ref_axis',(-0.5,0.,0.866025403784439));
#7110=DIRECTION('',(0.5,0.,-0.866025403784439));
#7111=DIRECTION('',(-0.5,0.,0.866025403784439));
#7112=DIRECTION('center_axis',(0.,1.,0.));
#7113=DIRECTION('ref_axis',(1.,0.,0.));
#7114=DIRECTION('center_axis',(0.,-1.,0.));
#7115=DIRECTION('ref_axis',(0.,0.,-1.));
#7116=DIRECTION('center_axis',(0.,1.,0.));
#7117=DIRECTION('ref_axis',(1.,0.,0.));
#7118=DIRECTION('center_axis',(0.,1.,0.));
#7119=DIRECTION('ref_axis',(1.,0.,0.));
#7120=DIRECTION('center_axis',(0.,1.,0.));
#7121=DIRECTION('ref_axis',(0.,0.,1.));
#7122=DIRECTION('center_axis',(0.,-1.,0.));
#7123=DIRECTION('ref_axis',(1.,0.,0.));
#7124=DIRECTION('center_axis',(0.,-1.,0.));
#7125=DIRECTION('ref_axis',(1.,0.,0.));
#7126=DIRECTION('center_axis',(0.,-1.,0.));
#7127=DIRECTION('ref_axis',(1.,0.,0.));
#7128=DIRECTION('',(0.707106781186548,0.707106781186547,8.65956056235493E-17));
#7129=DIRECTION('center_axis',(0.,-1.,0.));
#7130=DIRECTION('ref_axis',(1.,0.,0.));
#7131=DIRECTION('center_axis',(0.,-1.,0.));
#7132=DIRECTION('ref_axis',(1.,0.,0.));
#7133=DIRECTION('',(0.,1.,0.));
#7134=DIRECTION('center_axis',(0.,1.,0.));
#7135=DIRECTION('ref_axis',(1.,0.,0.));
#7136=DIRECTION('center_axis',(0.,-1.,0.));
#7137=DIRECTION('ref_axis',(1.,0.,0.));
#7138=DIRECTION('',(-0.707106781186547,0.707106781186548,-8.65956056235493E-17));
#7139=DIRECTION('center_axis',(0.,-1.,0.));
#7140=DIRECTION('ref_axis',(0.,0.,-1.));
#7141=DIRECTION('center_axis',(0.,-1.,0.));
#7142=DIRECTION('ref_axis',(1.,0.,0.));
#7143=DIRECTION('center_axis',(0.,1.,0.));
#7144=DIRECTION('ref_axis',(1.,0.,0.));
#7145=DIRECTION('center_axis',(0.,1.,0.));
#7146=DIRECTION('ref_axis',(1.,0.,0.));
#7147=DIRECTION('',(-0.447213595499958,0.894427190999916,-5.47678698264203E-17));
#7148=DIRECTION('center_axis',(0.,-1.,0.));
#7149=DIRECTION('ref_axis',(1.,0.,0.));
#7150=DIRECTION('',(0.,1.,0.));
#7151=DIRECTION('axis',(0.,0.,1.));
#7152=DIRECTION('refdir',(1.,0.,0.));
#7153=DIRECTION('axis',(0.,0.,1.));
#7154=DIRECTION('refdir',(1.,0.,0.));
#7155=DIRECTION('center_axis',(0.,1.,0.));
#7156=DIRECTION('ref_axis',(1.,0.,0.));
#7157=DIRECTION('center_axis',(0.,1.,0.));
#7158=DIRECTION('ref_axis',(1.,0.,0.));
#7159=DIRECTION('',(0.,1.,0.));
#7160=DIRECTION('center_axis',(0.,-1.,0.));
#7161=DIRECTION('ref_axis',(1.,0.,0.));
#7162=DIRECTION('center_axis',(0.,1.,0.));
#7163=DIRECTION('ref_axis',(1.,0.,0.));
#7164=DIRECTION('center_axis',(0.,1.,0.));
#7165=DIRECTION('ref_axis',(1.,0.,0.));
#7166=DIRECTION('',(0.,1.,0.));
#7167=DIRECTION('center_axis',(0.,-1.,0.));
#7168=DIRECTION('ref_axis',(1.,0.,0.));
#7169=DIRECTION('center_axis',(0.,1.,0.));
#7170=DIRECTION('ref_axis',(1.,0.,0.));
#7171=DIRECTION('',(0.,-1.,0.));
#7172=DIRECTION('center_axis',(0.,1.,0.));
#7173=DIRECTION('ref_axis',(1.,0.,0.));
#7174=DIRECTION('',(0.,1.,0.));
#7175=DIRECTION('center_axis',(0.,1.,0.));
#7176=DIRECTION('ref_axis',(1.,0.,0.));
#7177=DIRECTION('center_axis',(0.062254101962613,0.,-0.998060332238903));
#7178=DIRECTION('ref_axis',(-0.998060332238903,0.,-0.062254101962613));
#7179=DIRECTION('',(-0.998060332238903,0.,-0.062254101962613));
#7180=DIRECTION('',(0.,-1.,0.));
#7181=DIRECTION('',(-0.998060332238903,0.,-0.062254101962613));
#7182=DIRECTION('center_axis',(0.,1.,0.));
#7183=DIRECTION('ref_axis',(1.,0.,0.));
#7184=DIRECTION('',(0.998060332238903,0.,0.062254101962613));
#7185=DIRECTION('center_axis',(0.,1.,0.));
#7186=DIRECTION('ref_axis',(1.,0.,0.));
#7187=DIRECTION('center_axis',(-0.062254101962613,0.,0.998060332238903));
#7188=DIRECTION('ref_axis',(0.998060332238903,0.,0.062254101962613));
#7189=DIRECTION('',(0.998060332238903,0.,0.062254101962613));
#7190=DIRECTION('',(0.,1.,0.));
#7191=DIRECTION('center_axis',(0.,1.,0.));
#7192=DIRECTION('ref_axis',(-0.998060332238903,0.,-0.0622541019626133));
#7193=DIRECTION('center_axis',(0.,1.,0.));
#7194=DIRECTION('ref_axis',(1.,0.,0.));
#7195=DIRECTION('center_axis',(0.,1.,0.));
#7196=DIRECTION('ref_axis',(1.,0.,0.));
#7197=DIRECTION('',(0.,0.,1.));
#7198=DIRECTION('',(1.,0.,0.));
#7199=DIRECTION('axis',(0.,0.,1.));
#7200=DIRECTION('refdir',(1.,0.,0.));
#7201=DIRECTION('axis',(0.,0.,1.));
#7202=DIRECTION('refdir',(1.,0.,0.));
#7203=DIRECTION('center_axis',(1.,0.,0.));
#7204=DIRECTION('ref_axis',(0.,0.,-1.));
#7205=DIRECTION('center_axis',(1.,0.,0.));
#7206=DIRECTION('ref_axis',(0.,0.,-1.));
#7207=DIRECTION('',(1.,0.,0.));
#7208=DIRECTION('center_axis',(-1.,0.,0.));
#7209=DIRECTION('ref_axis',(0.,0.,-1.));
#7210=DIRECTION('center_axis',(1.,0.,0.));
#7211=DIRECTION('ref_axis',(0.,0.,-1.));
#7212=DIRECTION('center_axis',(0.,1.,0.));
#7213=DIRECTION('ref_axis',(1.,0.,0.));
#7214=DIRECTION('center_axis',(0.,1.,0.));
#7215=DIRECTION('ref_axis',(1.,0.,0.));
#7216=DIRECTION('',(0.,1.,0.));
#7217=DIRECTION('center_axis',(0.,-1.,0.));
#7218=DIRECTION('ref_axis',(1.,0.,0.));
#7219=DIRECTION('center_axis',(0.,1.,0.));
#7220=DIRECTION('ref_axis',(1.,0.,0.));
#7221=DIRECTION('center_axis',(0.,1.,0.));
#7222=DIRECTION('ref_axis',(1.,0.,0.));
#7223=DIRECTION('',(0.,1.,0.));
#7224=DIRECTION('center_axis',(0.,-1.,0.));
#7225=DIRECTION('ref_axis',(1.,0.,0.));
#7226=DIRECTION('center_axis',(-1.,0.,0.));
#7227=DIRECTION('ref_axis',(0.,0.,1.));
#7228=DIRECTION('',(0.,0.,1.));
#7229=DIRECTION('',(0.,1.,0.));
#7230=DIRECTION('',(0.,0.,-1.));
#7231=DIRECTION('',(0.,1.,0.));
#7232=DIRECTION('center_axis',(0.,1.,0.));
#7233=DIRECTION('ref_axis',(0.,0.,1.));
#7234=DIRECTION('',(-1.,0.,0.));
#7235=DIRECTION('',(0.,0.,1.));
#7236=DIRECTION('',(1.,0.,0.));
#7237=DIRECTION('',(0.,0.,-1.));
#7238=DIRECTION('center_axis',(0.,0.,-1.));
#7239=DIRECTION('ref_axis',(-1.,0.,0.));
#7240=DIRECTION('',(1.,0.,0.));
#7241=DIRECTION('',(0.,1.,0.));
#7242=DIRECTION('',(0.,1.,0.));
#7243=DIRECTION('',(1.,0.,0.));
#7244=DIRECTION('',(0.,1.,0.));
#7245=DIRECTION('',(-1.,0.,0.));
#7246=DIRECTION('center_axis',(0.,1.,0.));
#7247=DIRECTION('ref_axis',(1.,0.,0.));
#7248=DIRECTION('',(-1.,0.,0.));
#7249=DIRECTION('',(0.,0.,-1.));
#7250=DIRECTION('',(0.,0.,1.));
#7251=DIRECTION('center_axis',(-1.,0.,0.));
#7252=DIRECTION('ref_axis',(0.,0.,1.));
#7253=DIRECTION('',(0.,0.,-1.));
#7254=DIRECTION('',(0.,1.,0.));
#7255=DIRECTION('center_axis',(1.,0.,0.));
#7256=DIRECTION('ref_axis',(0.,0.,-1.));
#7257=DIRECTION('',(0.,1.,0.));
#7258=DIRECTION('center_axis',(1.,0.,0.));
#7259=DIRECTION('ref_axis',(0.,0.,-1.));
#7260=DIRECTION('center_axis',(0.,0.,1.));
#7261=DIRECTION('ref_axis',(1.,0.,0.));
#7262=DIRECTION('',(-1.,0.,0.));
#7263=DIRECTION('',(1.,0.,0.));
#7264=DIRECTION('',(0.,1.,0.));
#7265=DIRECTION('center_axis',(0.,1.,0.));
#7266=DIRECTION('ref_axis',(1.,0.,0.));
#7267=DIRECTION('center_axis',(-1.,0.,0.));
#7268=DIRECTION('ref_axis',(0.,0.,1.));
#7269=DIRECTION('',(0.,0.,1.));
#7270=DIRECTION('center_axis',(0.,1.,0.));
#7271=DIRECTION('ref_axis',(0.,0.,1.));
#7272=DIRECTION('center_axis',(1.,0.,0.));
#7273=DIRECTION('ref_axis',(0.,0.,-1.));
#7274=DIRECTION('center_axis',(1.,0.,0.));
#7275=DIRECTION('ref_axis',(0.,0.,-1.));
#7276=DIRECTION('',(-1.,0.,0.));
#7277=DIRECTION('center_axis',(1.,0.,0.));
#7278=DIRECTION('ref_axis',(0.,0.,-1.));
#7279=DIRECTION('axis',(0.,0.,1.));
#7280=DIRECTION('refdir',(1.,0.,0.));
#7281=DIRECTION('center_axis',(0.,-1.,0.));
#7282=DIRECTION('ref_axis',(1.,0.,0.));
#7283=DIRECTION('center_axis',(0.,1.,0.));
#7284=DIRECTION('ref_axis',(1.,0.,0.));
#7285=DIRECTION('',(0.,1.,0.));
#7286=DIRECTION('center_axis',(0.,-1.,0.));
#7287=DIRECTION('ref_axis',(1.,0.,0.));
#7288=DIRECTION('center_axis',(0.,1.,0.));
#7289=DIRECTION('ref_axis',(1.,0.,0.));
#7290=DIRECTION('center_axis',(0.,-1.,0.));
#7291=DIRECTION('ref_axis',(1.,0.,0.));
#7292=DIRECTION('',(-0.707106781186549,0.707106781186546,-8.65956056235496E-17));
#7293=DIRECTION('center_axis',(0.,-1.,0.));
#7294=DIRECTION('ref_axis',(0.,0.,-1.));
#7295=DIRECTION('center_axis',(0.,-1.,0.));
#7296=DIRECTION('ref_axis',(1.,0.,0.));
#7297=DIRECTION('center_axis',(0.,1.,0.));
#7298=DIRECTION('ref_axis',(1.,0.,0.));
#7299=DIRECTION('',(-0.866025403784439,-0.5,-1.06057523872491E-16));
#7300=DIRECTION('center_axis',(1.4792020664489E-16,0.,-1.));
#7301=DIRECTION('ref_axis',(-1.,0.,-1.4792020664489E-16));
#7302=DIRECTION('',(0.,1.,0.));
#7303=DIRECTION('',(-1.,0.,-1.4792020664489E-16));
#7304=DIRECTION('',(0.,1.,0.));
#7305=DIRECTION('center_axis',(0.866025403784439,0.,-0.5));
#7306=DIRECTION('ref_axis',(-0.5,0.,-0.866025403784439));
#7307=DIRECTION('',(0.,1.,0.));
#7308=DIRECTION('',(-0.5,0.,-0.866025403784439));
#7309=DIRECTION('center_axis',(0.866025403784439,0.,0.5));
#7310=DIRECTION('ref_axis',(0.5,0.,-0.866025403784439));
#7311=DIRECTION('',(0.,1.,0.));
#7312=DIRECTION('',(0.5,0.,-0.866025403784439));
#7313=DIRECTION('center_axis',(-2.95840413289779E-16,0.,1.));
#7314=DIRECTION('ref_axis',(1.,0.,2.95840413289779E-16));
#7315=DIRECTION('',(0.,1.,0.));
#7316=DIRECTION('',(1.,0.,2.95840413289779E-16));
#7317=DIRECTION('center_axis',(-0.866025403784439,0.,0.5));
#7318=DIRECTION('ref_axis',(0.5,0.,0.866025403784439));
#7319=DIRECTION('',(0.,1.,0.));
#7320=DIRECTION('',(0.5,0.,0.866025403784439));
#7321=DIRECTION('center_axis',(-0.866025403784439,0.,-0.5));
#7322=DIRECTION('ref_axis',(-0.5,0.,0.866025403784439));
#7323=DIRECTION('',(-0.5,0.,0.866025403784439));
#7324=DIRECTION('center_axis',(0.,1.,0.));
#7325=DIRECTION('ref_axis',(0.,0.,1.));
#7326=DIRECTION('center_axis',(0.,1.,0.));
#7327=DIRECTION('ref_axis',(1.,0.,0.));
#7328=DIRECTION('axis',(0.,0.,1.));
#7329=DIRECTION('refdir',(1.,0.,0.));
#7330=DIRECTION('center_axis',(0.,1.,0.));
#7331=DIRECTION('ref_axis',(1.,0.,0.));
#7332=DIRECTION('',(0.866025403784439,-0.5,1.06057523872491E-16));
#7333=DIRECTION('center_axis',(0.,-1.,0.));
#7334=DIRECTION('ref_axis',(1.,0.,0.));
#7335=DIRECTION('center_axis',(0.,-1.,0.));
#7336=DIRECTION('ref_axis',(1.,0.,0.));
#7337=DIRECTION('center_axis',(0.,1.,0.));
#7338=DIRECTION('ref_axis',(1.,0.,0.));
#7339=DIRECTION('',(-0.866025403784439,-0.5,-1.06057523872491E-16));
#7340=DIRECTION('center_axis',(1.4792020664489E-16,0.,-1.));
#7341=DIRECTION('ref_axis',(-1.,0.,-1.4792020664489E-16));
#7342=DIRECTION('',(0.,1.,0.));
#7343=DIRECTION('',(0.,1.,0.));
#7344=DIRECTION('center_axis',(-0.866025403784439,0.,-0.5));
#7345=DIRECTION('ref_axis',(-0.5,0.,0.866025403784439));
#7346=DIRECTION('',(0.,1.,0.));
#7347=DIRECTION('center_axis',(-0.866025403784439,0.,0.5));
#7348=DIRECTION('ref_axis',(0.5,0.,0.866025403784439));
#7349=DIRECTION('',(0.,1.,0.));
#7350=DIRECTION('center_axis',(0.,1.,0.));
#7351=DIRECTION('ref_axis',(1.,0.,0.));
#7352=DIRECTION('center_axis',(0.,1.,0.));
#7353=DIRECTION('ref_axis',(1.,0.,0.));
#7354=DIRECTION('',(0.,-1.,0.));
#7355=DIRECTION('center_axis',(0.,1.,0.));
#7356=DIRECTION('ref_axis',(1.,0.,0.));
#7357=DIRECTION('center_axis',(-2.95840413289779E-16,0.,1.));
#7358=DIRECTION('ref_axis',(1.,0.,2.95840413289779E-16));
#7359=DIRECTION('',(0.,1.,0.));
#7360=DIRECTION('center_axis',(0.866025403784439,0.,-0.5));
#7361=DIRECTION('ref_axis',(-0.5,0.,-0.866025403784439));
#7362=DIRECTION('',(0.,1.,0.));
#7363=DIRECTION('center_axis',(0.866025403784439,0.,0.5));
#7364=DIRECTION('ref_axis',(0.5,0.,-0.866025403784439));
#7365=DIRECTION('center_axis',(0.,1.,0.));
#7366=DIRECTION('ref_axis',(1.,0.,0.));
#7367=DIRECTION('center_axis',(0.,1.,0.));
#7368=DIRECTION('ref_axis',(1.,0.,0.));
#7369=DIRECTION('axis',(0.,0.,1.));
#7370=DIRECTION('refdir',(1.,0.,0.));
#7371=DIRECTION('center_axis',(0.,0.,1.));
#7372=DIRECTION('ref_axis',(1.,0.,0.));
#7373=DIRECTION('center_axis',(0.,0.,1.));
#7374=DIRECTION('ref_axis',(1.,0.,0.));
#7375=DIRECTION('',(0.,0.,-1.));
#7376=DIRECTION('center_axis',(0.,0.,1.));
#7377=DIRECTION('ref_axis',(1.,0.,0.));
#7378=DIRECTION('center_axis',(0.,0.,1.));
#7379=DIRECTION('ref_axis',(1.,0.,0.));
#7380=DIRECTION('center_axis',(0.,0.,1.));
#7381=DIRECTION('ref_axis',(1.,0.,0.));
#7382=DIRECTION('axis',(0.,0.,1.));
#7383=DIRECTION('refdir',(1.,0.,0.));
#7384=DIRECTION('center_axis',(1.,0.,0.));
#7385=DIRECTION('ref_axis',(0.,0.,-1.));
#7386=DIRECTION('',(1.,0.,0.));
#7387=DIRECTION('center_axis',(0.,1.,0.));
#7388=DIRECTION('ref_axis',(0.,0.,1.));
#7389=DIRECTION('center_axis',(0.,-1.,0.));
#7390=DIRECTION('ref_axis',(1.,0.,0.));
#7391=DIRECTION('center_axis',(0.,-1.,0.));
#7392=DIRECTION('ref_axis',(1.,0.,0.));
#7393=DIRECTION('center_axis',(0.,-1.,0.));
#7394=DIRECTION('ref_axis',(1.,0.,0.));
#7395=DIRECTION('',(0.707106781186547,0.707106781186548,8.65956056235493E-17));
#7396=DIRECTION('center_axis',(0.,-1.,0.));
#7397=DIRECTION('ref_axis',(1.,0.,0.));
#7398=DIRECTION('center_axis',(0.,-1.,0.));
#7399=DIRECTION('ref_axis',(1.,0.,0.));
#7400=DIRECTION('',(0.,1.,0.));
#7401=DIRECTION('center_axis',(0.,-1.,0.));
#7402=DIRECTION('ref_axis',(0.,0.,-1.));
#7403=DIRECTION('center_axis',(0.,-1.,0.));
#7404=DIRECTION('ref_axis',(1.,0.,0.));
#7405=DIRECTION('center_axis',(0.,-1.,0.));
#7406=DIRECTION('ref_axis',(1.,0.,0.));
#7407=DIRECTION('center_axis',(0.,-1.,0.));
#7408=DIRECTION('ref_axis',(1.,0.,0.));
#7409=DIRECTION('',(0.,1.,0.));
#7410=DIRECTION('',(0.,1.,0.));
#7411=DIRECTION('center_axis',(0.,1.,0.));
#7412=DIRECTION('ref_axis',(1.,0.,0.));
#7413=DIRECTION('center_axis',(0.,-1.,0.));
#7414=DIRECTION('ref_axis',(1.,0.,0.));
#7415=DIRECTION('',(-0.707106781186548,0.707106781186547,-8.65956056235494E-17));
#7416=DIRECTION('center_axis',(0.,-1.,0.));
#7417=DIRECTION('ref_axis',(0.,0.,-1.));
#7418=DIRECTION('axis',(0.,0.,1.));
#7419=DIRECTION('refdir',(1.,0.,0.));
#7420=DIRECTION('center_axis',(0.,1.,0.));
#7421=DIRECTION('ref_axis',(1.,0.,0.));
#7422=DIRECTION('center_axis',(0.,-1.,0.));
#7423=DIRECTION('ref_axis',(1.,0.,0.));
#7424=DIRECTION('',(0.,-1.,0.));
#7425=DIRECTION('center_axis',(0.,-1.,0.));
#7426=DIRECTION('ref_axis',(1.,0.,0.));
#7427=DIRECTION('center_axis',(0.,1.,0.));
#7428=DIRECTION('ref_axis',(1.,0.,0.));
#7429=DIRECTION('center_axis',(0.,1.,0.));
#7430=DIRECTION('ref_axis',(1.,0.,0.));
#7431=DIRECTION('',(0.,-1.,0.));
#7432=DIRECTION('center_axis',(0.,1.,0.));
#7433=DIRECTION('ref_axis',(1.,0.,0.));
#7434=DIRECTION('center_axis',(0.,1.,0.));
#7435=DIRECTION('ref_axis',(1.,0.,0.));
#7436=DIRECTION('center_axis',(0.,1.,0.));
#7437=DIRECTION('ref_axis',(1.,0.,0.));
#7438=DIRECTION('axis',(0.,0.,1.));
#7439=DIRECTION('refdir',(1.,0.,0.));
#7440=DIRECTION('center_axis',(0.,1.,0.));
#7441=DIRECTION('ref_axis',(1.,0.,0.));
#7442=DIRECTION('center_axis',(0.,-1.,0.));
#7443=DIRECTION('ref_axis',(1.,0.,0.));
#7444=DIRECTION('',(0.,-1.,0.));
#7445=DIRECTION('center_axis',(0.,-1.,0.));
#7446=DIRECTION('ref_axis',(1.,0.,0.));
#7447=DIRECTION('center_axis',(0.,1.,0.));
#7448=DIRECTION('ref_axis',(1.,0.,0.));
#7449=DIRECTION('center_axis',(0.,1.,0.));
#7450=DIRECTION('ref_axis',(1.,0.,0.));
#7451=DIRECTION('',(0.,-1.,0.));
#7452=DIRECTION('center_axis',(0.,1.,0.));
#7453=DIRECTION('ref_axis',(1.,0.,0.));
#7454=DIRECTION('center_axis',(0.,1.,0.));
#7455=DIRECTION('ref_axis',(1.,0.,0.));
#7456=DIRECTION('center_axis',(0.,1.,0.));
#7457=DIRECTION('ref_axis',(1.,0.,0.));
#7458=DIRECTION('axis',(0.,0.,1.));
#7459=DIRECTION('refdir',(1.,0.,0.));
#7460=DIRECTION('center_axis',(-1.,0.,0.));
#7461=DIRECTION('ref_axis',(0.,0.,1.));
#7462=DIRECTION('center_axis',(0.,-1.,1.38777878078145E-16));
#7463=DIRECTION('ref_axis',(0.,-1.38777878078145E-16,-1.));
#7464=DIRECTION('center_axis',(1.,0.,0.));
#7465=DIRECTION('ref_axis',(0.,0.,1.));
#7466=DIRECTION('center_axis',(0.,1.,0.));
#7467=DIRECTION('ref_axis',(1.,0.,0.));
#7468=DIRECTION('center_axis',(0.,-1.,0.));
#7469=DIRECTION('ref_axis',(1.,0.,0.));
#7470=DIRECTION('',(0.,0.,1.));
#7471=DIRECTION('center_axis',(1.,0.,0.));
#7472=DIRECTION('ref_axis',(0.,0.,1.));
#7473=DIRECTION('',(0.,-1.,0.));
#7474=DIRECTION('',(0.,0.,1.));
#7475=DIRECTION('',(0.,-1.,0.));
#7476=DIRECTION('center_axis',(0.,-1.,0.));
#7477=DIRECTION('ref_axis',(1.,0.,0.));
#7478=DIRECTION('center_axis',(0.,-1.,0.));
#7479=DIRECTION('ref_axis',(1.,0.,0.));
#7480=DIRECTION('',(0.,1.,0.));
#7481=DIRECTION('center_axis',(0.,-1.,0.));
#7482=DIRECTION('ref_axis',(1.,0.,0.));
#7483=DIRECTION('center_axis',(0.,1.,0.));
#7484=DIRECTION('ref_axis',(1.,0.,0.));
#7485=DIRECTION('',(0.,0.,1.));
#7486=DIRECTION('',(1.,0.,0.));
#7487=DIRECTION('',(0.,0.,1.));
#7488=DIRECTION('',(1.,0.,0.));
#7489=DIRECTION('',(0.,0.,1.));
#7490=DIRECTION('',(1.,0.,0.));
#7491=DIRECTION('',(0.,0.,1.));
#7492=DIRECTION('',(1.,0.,0.));
#7493=DIRECTION('',(0.,0.,1.));
#7494=DIRECTION('',(1.,0.,0.));
#7495=DIRECTION('',(0.,0.,1.));
#7496=DIRECTION('',(2.22044604925031E-16,1.,0.));
#7497=DIRECTION('',(0.,0.,1.));
#7498=DIRECTION('',(1.,0.,0.));
#7499=DIRECTION('',(0.,-1.,2.22044604925031E-16));
#7500=DIRECTION('',(1.,0.,0.));
#7501=DIRECTION('',(0.,-1.,2.22044604925031E-16));
#7502=DIRECTION('',(1.,0.,0.));
#7503=DIRECTION('',(0.,-1.,2.22044604925031E-16));
#7504=DIRECTION('',(1.,0.,0.));
#7505=DIRECTION('',(0.,-1.,2.22044604925031E-16));
#7506=DIRECTION('',(1.,0.,0.));
#7507=DIRECTION('',(0.,0.,1.));
#7508=DIRECTION('',(1.,0.,0.));
#7509=DIRECTION('',(0.,0.,1.));
#7510=DIRECTION('',(1.,0.,0.));
#7511=DIRECTION('',(0.,0.,1.));
#7512=DIRECTION('',(1.,0.,0.));
#7513=DIRECTION('',(0.,0.,1.));
#7514=DIRECTION('',(2.22044604925031E-16,1.,0.));
#7515=DIRECTION('',(0.,0.,1.));
#7516=DIRECTION('',(2.22044604925031E-16,-1.,0.));
#7517=DIRECTION('',(0.,0.,1.));
#7518=DIRECTION('',(2.22044604925031E-16,1.,0.));
#7519=DIRECTION('',(0.,0.,1.));
#7520=DIRECTION('',(2.22044604925031E-16,-1.,0.));
#7521=DIRECTION('',(0.,0.,1.));
#7522=DIRECTION('',(1.,0.,0.));
#7523=DIRECTION('',(0.,0.,1.));
#7524=DIRECTION('',(1.,0.,0.));
#7525=DIRECTION('',(0.,0.,1.));
#7526=DIRECTION('',(2.22044604925031E-16,-1.,0.));
#7527=DIRECTION('',(0.,0.,1.));
#7528=DIRECTION('',(2.22044604925031E-16,-1.,0.));
#7529=DIRECTION('',(0.,0.,1.));
#7530=DIRECTION('',(2.22044604925031E-16,1.,0.));
#7531=DIRECTION('',(0.,0.,1.));
#7532=DIRECTION('',(2.22044604925031E-16,1.,0.));
#7533=DIRECTION('',(0.,0.,1.));
#7534=DIRECTION('',(1.,0.,0.));
#7535=DIRECTION('',(0.,0.,1.));
#7536=DIRECTION('',(1.,0.,0.));
#7537=DIRECTION('',(0.,0.,1.));
#7538=DIRECTION('',(1.,0.,0.));
#7539=DIRECTION('',(0.,0.,1.));
#7540=DIRECTION('',(1.,0.,0.));
#7541=DIRECTION('',(0.,0.,1.));
#7542=DIRECTION('',(1.,0.,0.));
#7543=DIRECTION('',(0.,0.,1.));
#7544=DIRECTION('',(1.,0.,0.));
#7545=DIRECTION('',(0.,0.,1.));
#7546=DIRECTION('',(1.,0.,0.));
#7547=DIRECTION('',(0.,0.,1.));
#7548=DIRECTION('',(2.22044604925031E-16,1.,0.));
#7549=DIRECTION('',(0.,0.,1.));
#7550=DIRECTION('',(1.,0.,0.));
#7551=DIRECTION('',(0.,0.,1.));
#7552=DIRECTION('',(2.22044604925031E-16,-1.,0.));
#7553=DIRECTION('',(0.,0.,1.));
#7554=DIRECTION('',(2.22044604925031E-16,-1.,0.));
#7555=DIRECTION('',(1.,0.,2.22044604925031E-16));
#7556=DIRECTION('',(2.22044604925031E-16,0.,-1.));
#7557=DIRECTION('',(0.,0.,1.));
#7558=DIRECTION('',(1.,0.,0.));
#7559=DIRECTION('',(0.,0.,1.));
#7560=DIRECTION('',(1.,0.,0.));
#7561=DIRECTION('',(0.,0.,1.));
#7562=DIRECTION('',(1.,0.,0.));
#7563=DIRECTION('',(0.,0.,1.));
#7564=DIRECTION('',(1.,0.,0.));
#7565=DIRECTION('',(0.,0.,1.));
#7566=DIRECTION('',(2.22044604925031E-16,1.,0.));
#7567=DIRECTION('',(0.,0.,1.));
#7568=DIRECTION('',(1.,0.,0.));
#7569=DIRECTION('',(0.,0.,1.));
#7570=DIRECTION('',(1.,0.,0.));
#7571=DIRECTION('',(0.,0.,1.));
#7572=DIRECTION('',(1.,0.,0.));
#7573=DIRECTION('',(0.,0.,1.));
#7574=DIRECTION('',(1.,0.,0.));
#7575=CARTESIAN_POINT('',(0.,0.,0.));
#7576=CARTESIAN_POINT('',(0.,0.,0.));
#7577=CARTESIAN_POINT('',(0.,0.,0.));
#7578=CARTESIAN_POINT('Origin',(1.04595925965485,-0.4,6.42376977244362));
#7579=CARTESIAN_POINT('',(1.04595925965485,0.9,6.12376977244362));
#7580=CARTESIAN_POINT('',(1.04595925965485,1.25,6.12376977244362));
#7581=CARTESIAN_POINT('',(1.04595925965485,0.9,6.12376977244362));
#7582=CARTESIAN_POINT('',(1.04595925965485,0.9,6.72376977244362));
#7583=CARTESIAN_POINT('Origin',(1.04595925965485,0.9,6.42376977244362));
#7584=CARTESIAN_POINT('',(1.04595925965485,1.25,6.72376977244362));
#7585=CARTESIAN_POINT('',(1.04595925965485,0.9,6.72376977244362));
#7586=CARTESIAN_POINT('',(0.745959259654855,1.25,6.42376977244362));
#7587=CARTESIAN_POINT('Origin',(1.04595925965485,1.25,6.42376977244362));
#7588=CARTESIAN_POINT('',(0.745959259654855,-0.4,6.42376977244362));
#7589=CARTESIAN_POINT('',(0.745959259654855,-0.4,6.42376977244362));
#7590=CARTESIAN_POINT('Origin',(1.04595925965485,-0.4,6.42376977244362));
#7591=CARTESIAN_POINT('Origin',(1.04595925965485,1.25,6.42376977244362));
#7592=CARTESIAN_POINT('Origin',(1.04595925965485,-0.4,6.42376977244362));
#7593=CARTESIAN_POINT('Origin',(11.,1.25,0.));
#7594=CARTESIAN_POINT('',(7.4,1.25,6.72376977244362));
#7595=CARTESIAN_POINT('',(7.4,1.25,6.72376977244362));
#7596=CARTESIAN_POINT('',(7.4,1.25,0.6));
#7597=CARTESIAN_POINT('',(7.4,1.25,6.12376977244362));
#7598=CARTESIAN_POINT('',(11.,1.25,0.6));
#7599=CARTESIAN_POINT('',(11.,1.25,0.6));
#7600=CARTESIAN_POINT('',(11.,1.25,0.));
#7601=CARTESIAN_POINT('',(11.,1.25,0.));
#7602=CARTESIAN_POINT('',(-2.,1.25,0.));
#7603=CARTESIAN_POINT('',(11.,1.25,0.));
#7604=CARTESIAN_POINT('',(-2.,1.25,0.6));
#7605=CARTESIAN_POINT('',(-2.,1.25,0.));
#7606=CARTESIAN_POINT('',(6.8,1.25,0.6));
#7607=CARTESIAN_POINT('',(11.,1.25,0.6));
#7608=CARTESIAN_POINT('',(6.8,1.25,6.12376977244362));
#7609=CARTESIAN_POINT('',(6.8,1.25,6.42376977244362));
#7610=CARTESIAN_POINT('',(1.04595925965485,1.25,6.12376977244362));
#7611=CARTESIAN_POINT('Origin',(7.4,0.9,6.12376977244362));
#7612=CARTESIAN_POINT('',(6.8,0.9,6.12376977244362));
#7613=CARTESIAN_POINT('',(6.8,0.9,6.12376977244362));
#7614=CARTESIAN_POINT('',(1.04595925965485,0.9,6.12376977244362));
#7615=CARTESIAN_POINT('Origin',(1.04595925965485,0.9,6.72376977244362));
#7616=CARTESIAN_POINT('',(7.4,0.9,6.72376977244362));
#7617=CARTESIAN_POINT('',(7.4,0.9,6.72376977244362));
#7618=CARTESIAN_POINT('',(7.4,0.9,6.72376977244362));
#7619=CARTESIAN_POINT('Origin',(7.4,0.9,6.42376977244362));
#7620=CARTESIAN_POINT('',(7.4,0.9,0.6));
#7621=CARTESIAN_POINT('',(7.4,0.9,6.12376977244362));
#7622=CARTESIAN_POINT('',(7.4,0.45,0.6));
#7623=CARTESIAN_POINT('Origin',(6.8,0.9,0.5));
#7624=CARTESIAN_POINT('',(6.8,0.9,0.6));
#7625=CARTESIAN_POINT('',(6.8,0.45,0.6));
#7626=CARTESIAN_POINT('',(6.8,0.9,6.42376977244362));
#7627=CARTESIAN_POINT('Origin',(7.1,0.9,3.46188488622181));
#7628=CARTESIAN_POINT('',(5.8,0.9,0.6));
#7629=CARTESIAN_POINT('Origin',(4.5,0.,0.6));
#7630=CARTESIAN_POINT('',(-2.,-1.25,0.6));
#7631=CARTESIAN_POINT('',(-2.,1.25,0.6));
#7632=CARTESIAN_POINT('',(11.,-1.25,0.6));
#7633=CARTESIAN_POINT('',(-2.,-1.25,0.6));
#7634=CARTESIAN_POINT('',(11.,-1.25,0.6));
#7635=CARTESIAN_POINT('',(0.7,-0.5,0.6));
#7636=CARTESIAN_POINT('',(0.7,-0.9,0.6));
#7637=CARTESIAN_POINT('',(0.7,-0.45,0.6));
#7638=CARTESIAN_POINT('',(-0.7,-0.9,0.6));
#7639=CARTESIAN_POINT('',(2.25,-0.9,0.6));
#7640=CARTESIAN_POINT('',(-0.7,-0.5,0.6));
#7641=CARTESIAN_POINT('',(-0.7,-0.45,0.6));
#7642=CARTESIAN_POINT('',(2.25,-0.5,0.6));
#7643=CARTESIAN_POINT('',(0.7,0.9,0.6));
#7644=CARTESIAN_POINT('',(0.7,0.5,0.6));
#7645=CARTESIAN_POINT('',(0.7,0.25,0.6));
#7646=CARTESIAN_POINT('',(-0.7,0.5,0.6));
#7647=CARTESIAN_POINT('',(2.25,0.5,0.6));
#7648=CARTESIAN_POINT('',(-0.7,0.9,0.6));
#7649=CARTESIAN_POINT('',(-0.7,0.25,0.6));
#7650=CARTESIAN_POINT('',(2.25,0.9,0.6));
#7651=CARTESIAN_POINT('',(10.,0.9,0.6));
#7652=CARTESIAN_POINT('',(10.,-0.9,0.6));
#7653=CARTESIAN_POINT('',(10.,-0.45,0.6));
#7654=CARTESIAN_POINT('',(8.5,-0.9,0.6));
#7655=CARTESIAN_POINT('',(6.875,-0.9,0.6));
#7656=CARTESIAN_POINT('',(8.5,0.9,0.6));
#7657=CARTESIAN_POINT('',(8.5,-0.45,0.6));
#7658=CARTESIAN_POINT('',(6.875,0.9,0.6));
#7659=CARTESIAN_POINT('',(10.225,3.36777869765523E-17,0.6));
#7660=CARTESIAN_POINT('Origin',(10.5,0.,0.6));
#7661=CARTESIAN_POINT('',(-1.475,3.36777869765522E-17,0.6));
#7662=CARTESIAN_POINT('Origin',(-1.2,0.,0.6));
#7663=CARTESIAN_POINT('Origin',(-1.2,0.,-0.1));
#7664=CARTESIAN_POINT('',(-1.475,-3.36777869765522E-17,0.));
#7665=CARTESIAN_POINT('Origin',(-1.2,0.,0.));
#7666=CARTESIAN_POINT('',(-1.475,-3.36777869765522E-17,-0.1));
#7667=CARTESIAN_POINT('Origin',(10.5,0.,-0.1));
#7668=CARTESIAN_POINT('',(10.225,-3.36777869765523E-17,0.));
#7669=CARTESIAN_POINT('Origin',(10.5,0.,0.));
#7670=CARTESIAN_POINT('',(10.225,-3.36777869765523E-17,-0.1));
#7671=CARTESIAN_POINT('Origin',(8.4,0.,2.5));
#7672=CARTESIAN_POINT('',(8.5,-6.2456986756515E-17,3.01));
#7673=CARTESIAN_POINT('Origin',(8.5,0.,2.5));
#7674=CARTESIAN_POINT('',(10.,6.2456986756515E-17,3.01));
#7675=CARTESIAN_POINT('',(8.4,-6.2456986756515E-17,3.01));
#7676=CARTESIAN_POINT('Origin',(10.,0.,2.5));
#7677=CARTESIAN_POINT('Origin',(9.25,-0.9,2.));
#7678=CARTESIAN_POINT('',(10.,-0.9,3.5));
#7679=CARTESIAN_POINT('',(10.,-0.9,0.5));
#7680=CARTESIAN_POINT('',(8.5,-0.9,3.5));
#7681=CARTESIAN_POINT('',(10.,-0.9,3.5));
#7682=CARTESIAN_POINT('',(8.5,-0.9,3.5));
#7683=CARTESIAN_POINT('Origin',(10.,-0.9,3.5));
#7684=CARTESIAN_POINT('',(10.,0.9,3.5));
#7685=CARTESIAN_POINT('',(10.,0.9,0.5));
#7686=CARTESIAN_POINT('',(10.,-0.9,3.5));
#7687=CARTESIAN_POINT('Origin',(8.5,-0.9,0.5));
#7688=CARTESIAN_POINT('',(8.5,0.9,3.5));
#7689=CARTESIAN_POINT('',(8.5,-0.9,3.5));
#7690=CARTESIAN_POINT('',(8.5,0.9,3.5));
#7691=CARTESIAN_POINT('Origin',(8.5,-0.9,3.5));
#7692=CARTESIAN_POINT('',(10.,0.9,3.5));
#7693=CARTESIAN_POINT('Origin',(9.25,0.9,2.));
#7694=CARTESIAN_POINT('Origin',(0.,-1.,2.5));
#7695=CARTESIAN_POINT('',(-0.31,-0.9,2.5));
#7696=CARTESIAN_POINT('Origin',(0.,-0.9,2.5));
#7697=CARTESIAN_POINT('',(-0.31,-0.5,2.5));
#7698=CARTESIAN_POINT('',(-0.31,-1.,2.5));
#7699=CARTESIAN_POINT('Origin',(0.,-0.5,2.5));
#7700=CARTESIAN_POINT('Origin',(0.,-1.,2.5));
#7701=CARTESIAN_POINT('',(-0.31,0.5,2.5));
#7702=CARTESIAN_POINT('Origin',(0.,0.5,2.5));
#7703=CARTESIAN_POINT('',(-0.31,0.9,2.5));
#7704=CARTESIAN_POINT('',(-0.31,-1.,2.5));
#7705=CARTESIAN_POINT('Origin',(0.,0.9,2.5));
#7706=CARTESIAN_POINT('Origin',(0.,0.5,1.9));
#7707=CARTESIAN_POINT('',(0.7,0.5,3.3));
#7708=CARTESIAN_POINT('',(0.7,0.5,0.5));
#7709=CARTESIAN_POINT('',(-0.7,0.5,3.3));
#7710=CARTESIAN_POINT('',(0.7,0.5,3.3));
#7711=CARTESIAN_POINT('',(-0.7,0.5,3.3));
#7712=CARTESIAN_POINT('Origin',(0.7,0.5,3.3));
#7713=CARTESIAN_POINT('',(0.7,0.9,3.3));
#7714=CARTESIAN_POINT('',(0.7,0.9,0.5));
#7715=CARTESIAN_POINT('',(0.7,0.5,3.3));
#7716=CARTESIAN_POINT('Origin',(-0.7,0.5,0.5));
#7717=CARTESIAN_POINT('',(-0.7,0.9,3.3));
#7718=CARTESIAN_POINT('',(-0.7,0.5,3.3));
#7719=CARTESIAN_POINT('',(-0.7,0.9,3.3));
#7720=CARTESIAN_POINT('Origin',(-0.7,0.5,3.3));
#7721=CARTESIAN_POINT('',(0.7,0.9,3.3));
#7722=CARTESIAN_POINT('Origin',(0.,0.9,1.9));
#7723=CARTESIAN_POINT('Origin',(0.,-0.9,1.9));
#7724=CARTESIAN_POINT('',(0.7,-0.9,3.3));
#7725=CARTESIAN_POINT('',(0.7,-0.9,0.5));
#7726=CARTESIAN_POINT('',(-0.7,-0.9,3.3));
#7727=CARTESIAN_POINT('',(0.7,-0.9,3.3));
#7728=CARTESIAN_POINT('',(-0.7,-0.9,3.3));
#7729=CARTESIAN_POINT('Origin',(0.7,-0.9,3.3));
#7730=CARTESIAN_POINT('',(0.7,-0.5,3.3));
#7731=CARTESIAN_POINT('',(0.7,-0.5,0.5));
#7732=CARTESIAN_POINT('',(0.7,-0.9,3.3));
#7733=CARTESIAN_POINT('Origin',(-0.7,-0.9,0.5));
#7734=CARTESIAN_POINT('',(-0.7,-0.5,3.3));
#7735=CARTESIAN_POINT('',(-0.7,-0.9,3.3));
#7736=CARTESIAN_POINT('',(-0.7,-0.5,3.3));
#7737=CARTESIAN_POINT('Origin',(-0.7,-0.9,3.3));
#7738=CARTESIAN_POINT('',(0.7,-0.5,3.3));
#7739=CARTESIAN_POINT('Origin',(0.,-0.5,1.9));
#7740=CARTESIAN_POINT('Origin',(11.,-1.25,0.));
#7741=CARTESIAN_POINT('',(11.,-1.25,0.));
#7742=CARTESIAN_POINT('',(11.,-1.25,0.));
#7743=CARTESIAN_POINT('',(11.,-1.25,0.));
#7744=CARTESIAN_POINT('Origin',(-2.,-1.25,0.));
#7745=CARTESIAN_POINT('',(-2.,-1.25,0.));
#7746=CARTESIAN_POINT('',(-2.,-1.25,0.));
#7747=CARTESIAN_POINT('',(-2.,-1.25,0.));
#7748=CARTESIAN_POINT('Origin',(-2.,1.25,0.));
#7749=CARTESIAN_POINT('',(-2.,1.25,0.));
#7750=CARTESIAN_POINT('Origin',(4.5,0.,0.));
#7751=CARTESIAN_POINT('',(0.,0.,0.));
#7752=CARTESIAN_POINT('Origin',(17.3,0.,-0.8));
#7753=CARTESIAN_POINT('',(17.3,0.519615242270663,-0.5));
#7754=CARTESIAN_POINT('',(18.,0.519615242270663,-0.5));
#7755=CARTESIAN_POINT('',(17.3,0.519615242270663,-0.5));
#7756=CARTESIAN_POINT('',(17.3,-0.519615242270663,-0.5));
#7757=CARTESIAN_POINT('Origin',(17.3,0.,-0.8));
#7758=CARTESIAN_POINT('',(18.,-0.519615242270663,-0.5));
#7759=CARTESIAN_POINT('',(17.3,-0.519615242270663,-0.5));
#7760=CARTESIAN_POINT('Origin',(18.,0.,-0.8));
#7761=CARTESIAN_POINT('Origin',(17.3,0.,-0.8));
#7762=CARTESIAN_POINT('',(17.3,0.,-0.5));
#7763=CARTESIAN_POINT('Origin',(18.,0.,1.75));
#7764=CARTESIAN_POINT('',(18.,-1.25,-0.5));
#7765=CARTESIAN_POINT('',(18.,-1.25,-0.5));
#7766=CARTESIAN_POINT('',(18.,-1.25,5.));
#7767=CARTESIAN_POINT('',(18.,-1.25,5.));
#7768=CARTESIAN_POINT('',(18.,1.25,5.));
#7769=CARTESIAN_POINT('',(18.,1.25,5.));
#7770=CARTESIAN_POINT('',(18.,1.25,-0.5));
#7771=CARTESIAN_POINT('',(18.,1.25,-1.5));
#7772=CARTESIAN_POINT('',(18.,-1.25,-0.5));
#7773=CARTESIAN_POINT('',(18.,-4.04133443718627E-17,4.33));
#7774=CARTESIAN_POINT('Origin',(18.,0.,4.));
#7775=CARTESIAN_POINT('',(18.,-4.04133443718626E-17,-0.47));
#7776=CARTESIAN_POINT('Origin',(18.,0.,-0.8));
#7777=CARTESIAN_POINT('Origin',(17.9,0.,-0.8));
#7778=CARTESIAN_POINT('',(18.8,4.04133443718626E-17,-0.47));
#7779=CARTESIAN_POINT('',(17.9,-4.04133443718626E-17,-0.47));
#7780=CARTESIAN_POINT('Origin',(18.8,0.,-0.8));
#7781=CARTESIAN_POINT('Origin',(17.9,0.,4.));
#7782=CARTESIAN_POINT('',(18.8,4.04133443718627E-17,4.33));
#7783=CARTESIAN_POINT('',(17.9,-4.04133443718627E-17,4.33));
#7784=CARTESIAN_POINT('Origin',(18.8,0.,4.));
#7785=CARTESIAN_POINT('Origin',(8.,0.,-0.5));
#7786=CARTESIAN_POINT('',(11.,1.25,-0.5));
#7787=CARTESIAN_POINT('',(18.,1.25,-0.5));
#7788=CARTESIAN_POINT('',(11.,-1.25,-0.5));
#7789=CARTESIAN_POINT('',(11.,-0.625,-0.5));
#7790=CARTESIAN_POINT('',(-2.,-1.25,-0.5));
#7791=CARTESIAN_POINT('Origin',(10.5,0.,-1.2));
#7792=CARTESIAN_POINT('',(10.29,-2.57175827820945E-17,-1.2));
#7793=CARTESIAN_POINT('Origin',(10.5,0.,-1.2));
#7794=CARTESIAN_POINT('',(10.29,2.57175827820945E-17,0.));
#7795=CARTESIAN_POINT('',(10.29,-2.57175827820945E-17,-1.2));
#7796=CARTESIAN_POINT('Origin',(10.5,0.,0.));
#7797=CARTESIAN_POINT('Origin',(10.5,0.,-1.2));
#7798=CARTESIAN_POINT('Origin',(11.,-1.25,-0.5));
#7799=CARTESIAN_POINT('',(11.,1.25,0.));
#7800=CARTESIAN_POINT('',(11.,1.25,-0.5));
#7801=CARTESIAN_POINT('',(11.,-1.25,0.));
#7802=CARTESIAN_POINT('',(11.,-1.25,0.));
#7803=CARTESIAN_POINT('',(11.,-1.25,-0.5));
#7804=CARTESIAN_POINT('Origin',(10.,1.25,-0.5));
#7805=CARTESIAN_POINT('',(10.,-1.25,-0.5));
#7806=CARTESIAN_POINT('',(10.,1.25,-0.5));
#7807=CARTESIAN_POINT('',(10.,0.625,-0.5));
#7808=CARTESIAN_POINT('',(10.,-1.25,0.));
#7809=CARTESIAN_POINT('',(10.,-1.25,-0.5));
#7810=CARTESIAN_POINT('',(10.,1.25,0.));
#7811=CARTESIAN_POINT('',(10.,1.25,0.));
#7812=CARTESIAN_POINT('',(10.,1.25,-0.5));
#7813=CARTESIAN_POINT('Origin',(10.5,0.,0.));
#7814=CARTESIAN_POINT('',(10.,-1.25,0.));
#7815=CARTESIAN_POINT('',(11.,1.25,0.));
#7816=CARTESIAN_POINT('Origin',(8.,0.,-0.5));
#7817=CARTESIAN_POINT('',(-0.7,1.25,-0.5));
#7818=CARTESIAN_POINT('',(18.,1.25,-0.5));
#7819=CARTESIAN_POINT('',(-0.7,-1.25,-0.5));
#7820=CARTESIAN_POINT('',(-0.7,-0.625,-0.5));
#7821=CARTESIAN_POINT('',(-2.,-1.25,-0.5));
#7822=CARTESIAN_POINT('Origin',(-1.2,0.,-1.2));
#7823=CARTESIAN_POINT('',(-1.41,-2.57175827820944E-17,-1.2));
#7824=CARTESIAN_POINT('Origin',(-1.2,0.,-1.2));
#7825=CARTESIAN_POINT('',(-1.41,2.57175827820944E-17,0.));
#7826=CARTESIAN_POINT('',(-1.41,-2.57175827820944E-17,-1.2));
#7827=CARTESIAN_POINT('Origin',(-1.2,0.,0.));
#7828=CARTESIAN_POINT('Origin',(-1.2,0.,-1.2));
#7829=CARTESIAN_POINT('Origin',(-0.7,-1.25,-0.5));
#7830=CARTESIAN_POINT('',(-0.7,1.25,0.));
#7831=CARTESIAN_POINT('',(-0.7,1.25,-0.5));
#7832=CARTESIAN_POINT('',(-0.7,-1.25,0.));
#7833=CARTESIAN_POINT('',(-0.7,-1.25,0.));
#7834=CARTESIAN_POINT('',(-0.7,-1.25,-0.5));
#7835=CARTESIAN_POINT('Origin',(-1.7,1.25,-0.5));
#7836=CARTESIAN_POINT('',(-1.7,-1.25,-0.5));
#7837=CARTESIAN_POINT('',(-1.7,1.25,-0.5));
#7838=CARTESIAN_POINT('',(-1.7,0.625,-0.5));
#7839=CARTESIAN_POINT('',(-1.7,-1.25,0.));
#7840=CARTESIAN_POINT('',(-1.7,-1.25,-0.5));
#7841=CARTESIAN_POINT('',(-1.7,1.25,0.));
#7842=CARTESIAN_POINT('',(-1.7,1.25,0.));
#7843=CARTESIAN_POINT('',(-1.7,1.25,-0.5));
#7844=CARTESIAN_POINT('Origin',(-1.2,0.,0.));
#7845=CARTESIAN_POINT('',(-1.7,-1.25,0.));
#7846=CARTESIAN_POINT('',(-0.7,1.25,0.));
#7847=CARTESIAN_POINT('Origin',(8.,0.,-0.5));
#7848=CARTESIAN_POINT('',(-2.,1.25,-0.5));
#7849=CARTESIAN_POINT('',(18.,1.25,-0.5));
#7850=CARTESIAN_POINT('',(-2.,-1.25,-0.5));
#7851=CARTESIAN_POINT('',(-2.,1.25,-0.5));
#7852=CARTESIAN_POINT('',(-2.,-1.25,-0.5));
#7853=CARTESIAN_POINT('Origin',(18.,1.25,5.));
#7854=CARTESIAN_POINT('',(18.8,-1.25,5.));
#7855=CARTESIAN_POINT('',(18.,-1.25,5.));
#7856=CARTESIAN_POINT('',(18.8,1.25,5.));
#7857=CARTESIAN_POINT('',(18.8,1.25,5.));
#7858=CARTESIAN_POINT('',(18.,1.25,5.));
#7859=CARTESIAN_POINT('Origin',(18.8,0.,1.75));
#7860=CARTESIAN_POINT('',(18.8,-1.25,-1.5));
#7861=CARTESIAN_POINT('',(18.8,-1.25,5.));
#7862=CARTESIAN_POINT('',(18.8,1.25,-1.5));
#7863=CARTESIAN_POINT('',(18.8,-1.25,-1.5));
#7864=CARTESIAN_POINT('',(18.8,1.25,-1.5));
#7865=CARTESIAN_POINT('Origin',(18.,1.25,-1.5));
#7866=CARTESIAN_POINT('',(-2.,1.25,-1.5));
#7867=CARTESIAN_POINT('',(18.,1.25,-1.5));
#7868=CARTESIAN_POINT('',(-2.,1.25,-1.5));
#7869=CARTESIAN_POINT('Origin',(-2.,-1.25,-1.5));
#7870=CARTESIAN_POINT('',(-2.,-1.25,-1.5));
#7871=CARTESIAN_POINT('',(-2.,-1.25,-1.5));
#7872=CARTESIAN_POINT('',(-2.,-1.25,-1.5));
#7873=CARTESIAN_POINT('Origin',(-2.,1.25,-1.5));
#7874=CARTESIAN_POINT('',(-2.,1.25,-1.5));
#7875=CARTESIAN_POINT('Origin',(8.,0.,-1.5));
#7876=CARTESIAN_POINT('',(0.,0.,0.));
#7877=CARTESIAN_POINT('Origin',(0.,0.09,0.));
#7878=CARTESIAN_POINT('',(-0.285,0.1,3.49024337756996E-17));
#7879=CARTESIAN_POINT('Origin',(0.,0.1,0.));
#7880=CARTESIAN_POINT('',(-0.265,0.08,-3.24531401774049E-17));
#7881=CARTESIAN_POINT('',(-0.275,0.09,3.36777869765522E-17));
#7882=CARTESIAN_POINT('Origin',(0.,0.08,0.));
#7883=CARTESIAN_POINT('Origin',(0.,0.,0.));
#7884=CARTESIAN_POINT('',(-0.265,0.,3.24531401774049E-17));
#7885=CARTESIAN_POINT('',(-0.265,0.,3.24531401774049E-17));
#7886=CARTESIAN_POINT('Origin',(0.,0.,0.));
#7887=CARTESIAN_POINT('Origin',(0.,0.1,0.));
#7888=CARTESIAN_POINT('',(-0.5,0.1,6.12323399573677E-17));
#7889=CARTESIAN_POINT('Origin',(0.,0.1,0.));
#7890=CARTESIAN_POINT('Origin',(0.,0.,0.));
#7891=CARTESIAN_POINT('',(-0.5,0.,6.12323399573677E-17));
#7892=CARTESIAN_POINT('',(-0.5,0.,6.12323399573677E-17));
#7893=CARTESIAN_POINT('Origin',(0.,0.,0.));
#7894=CARTESIAN_POINT('Origin',(0.,0.,0.));
#7895=CARTESIAN_POINT('',(0.,0.,0.));
#7896=CARTESIAN_POINT('Origin',(0.115470053837925,-0.5,-0.2));
#7897=CARTESIAN_POINT('',(0.23094010767585,-0.5,0.));
#7898=CARTESIAN_POINT('',(0.115470053837925,-0.5,-0.2));
#7899=CARTESIAN_POINT('',(0.23094010767585,-0.5,0.));
#7900=CARTESIAN_POINT('',(0.115470053837925,-0.8,-0.2));
#7901=CARTESIAN_POINT('',(0.115470053837925,-0.5,-0.2));
#7902=CARTESIAN_POINT('',(0.23094010767585,-0.8,0.));
#7903=CARTESIAN_POINT('',(0.23094010767585,-0.8,0.));
#7904=CARTESIAN_POINT('',(0.23094010767585,-0.5,0.));
#7905=CARTESIAN_POINT('Origin',(-0.115470053837925,-0.5,-0.2));
#7906=CARTESIAN_POINT('',(-0.115470053837925,-0.5,-0.2));
#7907=CARTESIAN_POINT('',(0.115470053837925,-0.5,-0.2));
#7908=CARTESIAN_POINT('',(-0.115470053837925,-0.8,-0.2));
#7909=CARTESIAN_POINT('',(-0.115470053837925,-0.5,-0.2));
#7910=CARTESIAN_POINT('',(0.115470053837925,-0.8,-0.2));
#7911=CARTESIAN_POINT('Origin',(-0.23094010767585,-0.5,-2.77555756156289E-17));
#7912=CARTESIAN_POINT('',(-0.23094010767585,-0.5,-2.82820063659975E-17));
#7913=CARTESIAN_POINT('',(-0.115470053837925,-0.5,-0.2));
#7914=CARTESIAN_POINT('',(-0.23094010767585,-0.8,-2.77555756156289E-17));
#7915=CARTESIAN_POINT('',(-0.23094010767585,-0.5,-2.82820063659975E-17));
#7916=CARTESIAN_POINT('',(-0.115470053837925,-0.8,-0.2));
#7917=CARTESIAN_POINT('Origin',(-0.115470053837925,-0.5,0.2));
#7918=CARTESIAN_POINT('',(-0.115470053837925,-0.5,0.2));
#7919=CARTESIAN_POINT('',(-0.23094010767585,-0.5,-2.82820063659975E-17));
#7920=CARTESIAN_POINT('',(-0.115470053837925,-0.8,0.2));
#7921=CARTESIAN_POINT('',(-0.115470053837925,-0.5,0.2));
#7922=CARTESIAN_POINT('',(-0.23094010767585,-0.8,-2.82820063659975E-17));
#7923=CARTESIAN_POINT('Origin',(0.115470053837925,-0.5,0.2));
#7924=CARTESIAN_POINT('',(0.115470053837925,-0.5,0.2));
#7925=CARTESIAN_POINT('',(-0.115470053837925,-0.5,0.2));
#7926=CARTESIAN_POINT('',(0.115470053837925,-0.8,0.2));
#7927=CARTESIAN_POINT('',(0.115470053837925,-0.5,0.2));
#7928=CARTESIAN_POINT('',(-0.115470053837925,-0.8,0.2));
#7929=CARTESIAN_POINT('Origin',(0.23094010767585,-0.5,0.));
#7930=CARTESIAN_POINT('',(0.115470053837925,-0.5,0.2));
#7931=CARTESIAN_POINT('',(0.115470053837925,-0.8,0.2));
#7932=CARTESIAN_POINT('Origin',(0.,-0.5,0.));
#7933=CARTESIAN_POINT('Origin',(0.,-0.8,0.));
#7934=CARTESIAN_POINT('Origin',(0.,-1.4,0.));
#7935=CARTESIAN_POINT('',(-0.24505,-1.4,3.00099698131059E-17));
#7936=CARTESIAN_POINT('Origin',(0.,-1.4,0.));
#7937=CARTESIAN_POINT('Origin',(0.375,0.5,0.));
#7938=CARTESIAN_POINT('',(-0.375,0.5,-4.59242549680257E-17));
#7939=CARTESIAN_POINT('Origin',(0.,0.5,0.));
#7940=CARTESIAN_POINT('Origin',(0.,0.475,0.));
#7941=CARTESIAN_POINT('',(-0.425,0.45,-5.20474889637625E-17));
#7942=CARTESIAN_POINT('Origin',(0.,0.45,0.));
#7943=CARTESIAN_POINT('',(-0.4,0.475,-4.89858719658941E-17));
#7944=CARTESIAN_POINT('Origin',(0.,0.24,0.));
#7945=CARTESIAN_POINT('',(-0.425,0.0299999999999998,-5.20474889637625E-17));
#7946=CARTESIAN_POINT('Origin',(0.,0.0299999999999998,0.));
#7947=CARTESIAN_POINT('',(-0.425,0.24,-5.20474889637625E-17));
#7948=CARTESIAN_POINT('Origin',(0.,0.0150000000000001,0.));
#7949=CARTESIAN_POINT('',(-0.395,4.85722573273506E-17,-4.83735485663204E-17));
#7950=CARTESIAN_POINT('Origin',(0.,0.,0.));
#7951=CARTESIAN_POINT('',(-0.41,0.0150000000000001,-5.02105187650415E-17));
#7952=CARTESIAN_POINT('Origin',(0.27,0.,0.));
#7953=CARTESIAN_POINT('',(-0.27,0.,-3.30654635769785E-17));
#7954=CARTESIAN_POINT('Origin',(0.,0.,0.));
#7955=CARTESIAN_POINT('Origin',(0.,-0.02,0.));
#7956=CARTESIAN_POINT('',(-0.24505,-0.0498999999999999,3.00099698131059E-17));
#7957=CARTESIAN_POINT('Origin',(0.,-0.0498999999999999,0.));
#7958=CARTESIAN_POINT('',(-0.26,-0.02,-3.18408167778312E-17));
#7959=CARTESIAN_POINT('Origin',(0.,-0.995,0.));
#7960=CARTESIAN_POINT('',(-0.24505,-0.995,-3.00099698131059E-17));
#7961=CARTESIAN_POINT('',(0.,0.,0.));
#7962=CARTESIAN_POINT('Origin',(18.7,-2.5,7.));
#7963=CARTESIAN_POINT('',(18.8,-2.5,7.3));
#7964=CARTESIAN_POINT('Origin',(18.8,-2.5,7.));
#7965=CARTESIAN_POINT('',(20.3,-2.5,7.3));
#7966=CARTESIAN_POINT('',(18.7,-2.5,7.3));
#7967=CARTESIAN_POINT('Origin',(20.3,-2.5,7.));
#7968=CARTESIAN_POINT('Origin',(18.7,2.5,7.));
#7969=CARTESIAN_POINT('',(18.8,2.5,7.3));
#7970=CARTESIAN_POINT('Origin',(18.8,2.5,7.));
#7971=CARTESIAN_POINT('',(20.3,2.5,7.3));
#7972=CARTESIAN_POINT('',(18.7,2.5,7.3));
#7973=CARTESIAN_POINT('Origin',(20.3,2.5,7.));
#7974=CARTESIAN_POINT('Origin',(18.7,6.5,-2.));
#7975=CARTESIAN_POINT('',(18.8,6.5,-1.67));
#7976=CARTESIAN_POINT('Origin',(18.8,6.5,-2.));
#7977=CARTESIAN_POINT('',(20.3,6.5,-1.67));
#7978=CARTESIAN_POINT('',(18.7,6.5,-1.67));
#7979=CARTESIAN_POINT('Origin',(20.3,6.5,-2.));
#7980=CARTESIAN_POINT('Origin',(18.7,-6.5,11.));
#7981=CARTESIAN_POINT('',(18.8,-6.5,11.33));
#7982=CARTESIAN_POINT('Origin',(18.8,-6.5,11.));
#7983=CARTESIAN_POINT('',(20.3,-6.5,11.33));
#7984=CARTESIAN_POINT('',(18.7,-6.5,11.33));
#7985=CARTESIAN_POINT('Origin',(20.3,-6.5,11.));
#7986=CARTESIAN_POINT('Origin',(18.7,-6.5,-2.));
#7987=CARTESIAN_POINT('',(18.8,-6.5,-1.67));
#7988=CARTESIAN_POINT('Origin',(18.8,-6.5,-2.));
#7989=CARTESIAN_POINT('',(20.3,-6.5,-1.67));
#7990=CARTESIAN_POINT('',(18.7,-6.5,-1.67));
#7991=CARTESIAN_POINT('Origin',(20.3,-6.5,-2.));
#7992=CARTESIAN_POINT('Origin',(18.7,6.5,11.));
#7993=CARTESIAN_POINT('',(18.8,6.5,11.33));
#7994=CARTESIAN_POINT('Origin',(18.8,6.5,11.));
#7995=CARTESIAN_POINT('',(20.3,6.5,11.33));
#7996=CARTESIAN_POINT('',(18.7,6.5,11.33));
#7997=CARTESIAN_POINT('Origin',(20.3,6.5,11.));
#7998=CARTESIAN_POINT('Origin',(18.7,0.,-0.8));
#7999=CARTESIAN_POINT('',(18.8,-4.04133443718626E-17,-0.47));
#8000=CARTESIAN_POINT('Origin',(18.8,0.,-0.8));
#8001=CARTESIAN_POINT('',(20.3,4.04133443718626E-17,-0.47));
#8002=CARTESIAN_POINT('',(18.7,-4.04133443718626E-17,-0.47));
#8003=CARTESIAN_POINT('Origin',(20.3,0.,-0.8));
#8004=CARTESIAN_POINT('Origin',(18.7,0.,4.));
#8005=CARTESIAN_POINT('',(18.8,-4.04133443718627E-17,4.33));
#8006=CARTESIAN_POINT('Origin',(18.8,0.,4.));
#8007=CARTESIAN_POINT('',(20.3,4.04133443718627E-17,4.33));
#8008=CARTESIAN_POINT('',(18.7,-4.04133443718627E-17,4.33));
#8009=CARTESIAN_POINT('Origin',(20.3,0.,4.));
#8010=CARTESIAN_POINT('Origin',(18.7,5.,7.));
#8011=CARTESIAN_POINT('',(18.8,5.,7.34));
#8012=CARTESIAN_POINT('Origin',(18.8,5.,7.));
#8013=CARTESIAN_POINT('',(20.3,5.,7.34));
#8014=CARTESIAN_POINT('',(18.7,5.,7.34));
#8015=CARTESIAN_POINT('Origin',(20.3,5.,7.));
#8016=CARTESIAN_POINT('Origin',(18.7,5.,2.));
#8017=CARTESIAN_POINT('',(18.8,5.,2.34));
#8018=CARTESIAN_POINT('Origin',(18.8,5.,2.));
#8019=CARTESIAN_POINT('',(20.3,5.,2.34));
#8020=CARTESIAN_POINT('',(18.7,5.,2.34));
#8021=CARTESIAN_POINT('Origin',(20.3,5.,2.));
#8022=CARTESIAN_POINT('Origin',(18.7,2.5,9.5));
#8023=CARTESIAN_POINT('',(18.8,2.5,9.84));
#8024=CARTESIAN_POINT('Origin',(18.8,2.5,9.5));
#8025=CARTESIAN_POINT('',(20.3,2.5,9.84));
#8026=CARTESIAN_POINT('',(18.7,2.5,9.84));
#8027=CARTESIAN_POINT('Origin',(20.3,2.5,9.5));
#8028=CARTESIAN_POINT('Origin',(18.7,2.5,2.));
#8029=CARTESIAN_POINT('',(18.8,2.5,2.34));
#8030=CARTESIAN_POINT('Origin',(18.8,2.5,2.));
#8031=CARTESIAN_POINT('',(20.3,2.5,2.34));
#8032=CARTESIAN_POINT('',(18.7,2.5,2.34));
#8033=CARTESIAN_POINT('Origin',(20.3,2.5,2.));
#8034=CARTESIAN_POINT('Origin',(18.7,0.,9.5));
#8035=CARTESIAN_POINT('',(18.8,-4.163799117101E-17,9.84));
#8036=CARTESIAN_POINT('Origin',(18.8,0.,9.5));
#8037=CARTESIAN_POINT('',(20.3,4.163799117101E-17,9.84));
#8038=CARTESIAN_POINT('',(18.7,-4.163799117101E-17,9.84));
#8039=CARTESIAN_POINT('Origin',(20.3,0.,9.5));
#8040=CARTESIAN_POINT('Origin',(18.7,0.,7.));
#8041=CARTESIAN_POINT('',(18.8,-4.163799117101E-17,7.34));
#8042=CARTESIAN_POINT('Origin',(18.8,0.,7.));
#8043=CARTESIAN_POINT('',(20.3,4.163799117101E-17,7.34));
#8044=CARTESIAN_POINT('',(18.7,-4.163799117101E-17,7.34));
#8045=CARTESIAN_POINT('Origin',(20.3,0.,7.));
#8046=CARTESIAN_POINT('Origin',(18.7,-2.5,4.5));
#8047=CARTESIAN_POINT('',(18.8,-2.5,4.84));
#8048=CARTESIAN_POINT('Origin',(18.8,-2.5,4.5));
#8049=CARTESIAN_POINT('',(20.3,-2.5,4.84));
#8050=CARTESIAN_POINT('',(18.7,-2.5,4.84));
#8051=CARTESIAN_POINT('Origin',(20.3,-2.5,4.5));
#8052=CARTESIAN_POINT('Origin',(18.7,-2.5,-0.5));
#8053=CARTESIAN_POINT('',(18.8,-2.5,-0.16));
#8054=CARTESIAN_POINT('Origin',(18.8,-2.5,-0.5));
#8055=CARTESIAN_POINT('',(20.3,-2.5,-0.16));
#8056=CARTESIAN_POINT('',(18.7,-2.5,-0.16));
#8057=CARTESIAN_POINT('Origin',(20.3,-2.5,-0.5));
#8058=CARTESIAN_POINT('Origin',(18.7,-5.,7.));
#8059=CARTESIAN_POINT('',(18.8,-5.,7.34));
#8060=CARTESIAN_POINT('Origin',(18.8,-5.,7.));
#8061=CARTESIAN_POINT('',(20.3,-5.,7.34));
#8062=CARTESIAN_POINT('',(18.7,-5.,7.34));
#8063=CARTESIAN_POINT('Origin',(20.3,-5.,7.));
#8064=CARTESIAN_POINT('Origin',(18.7,-5.,2.));
#8065=CARTESIAN_POINT('',(18.8,-5.,2.34));
#8066=CARTESIAN_POINT('Origin',(18.8,-5.,2.));
#8067=CARTESIAN_POINT('',(20.3,-5.,2.34));
#8068=CARTESIAN_POINT('',(18.7,-5.,2.34));
#8069=CARTESIAN_POINT('Origin',(20.3,-5.,2.));
#8070=CARTESIAN_POINT('Origin',(18.7,-5.,4.5));
#8071=CARTESIAN_POINT('',(18.8,-5.,4.84));
#8072=CARTESIAN_POINT('Origin',(18.8,-5.,4.5));
#8073=CARTESIAN_POINT('',(20.3,-5.,4.84));
#8074=CARTESIAN_POINT('',(18.7,-5.,4.84));
#8075=CARTESIAN_POINT('Origin',(20.3,-5.,4.5));
#8076=CARTESIAN_POINT('Origin',(18.7,-5.,9.5));
#8077=CARTESIAN_POINT('',(18.8,-5.,9.84));
#8078=CARTESIAN_POINT('Origin',(18.8,-5.,9.5));
#8079=CARTESIAN_POINT('',(20.3,-5.,9.84));
#8080=CARTESIAN_POINT('',(18.7,-5.,9.84));
#8081=CARTESIAN_POINT('Origin',(20.3,-5.,9.5));
#8082=CARTESIAN_POINT('Origin',(18.7,-2.5,2.));
#8083=CARTESIAN_POINT('',(18.8,-2.5,2.34));
#8084=CARTESIAN_POINT('Origin',(18.8,-2.5,2.));
#8085=CARTESIAN_POINT('',(20.3,-2.5,2.34));
#8086=CARTESIAN_POINT('',(18.7,-2.5,2.34));
#8087=CARTESIAN_POINT('Origin',(20.3,-2.5,2.));
#8088=CARTESIAN_POINT('Origin',(18.7,-2.5,9.5));
#8089=CARTESIAN_POINT('',(18.8,-2.5,9.84));
#8090=CARTESIAN_POINT('Origin',(18.8,-2.5,9.5));
#8091=CARTESIAN_POINT('',(20.3,-2.5,9.84));
#8092=CARTESIAN_POINT('',(18.7,-2.5,9.84));
#8093=CARTESIAN_POINT('Origin',(20.3,-2.5,9.5));
#8094=CARTESIAN_POINT('Origin',(18.7,-5.,-0.5));
#8095=CARTESIAN_POINT('',(18.8,-5.,-0.16));
#8096=CARTESIAN_POINT('Origin',(18.8,-5.,-0.5));
#8097=CARTESIAN_POINT('',(20.3,-5.,-0.16));
#8098=CARTESIAN_POINT('',(18.7,-5.,-0.16));
#8099=CARTESIAN_POINT('Origin',(20.3,-5.,-0.5));
#8100=CARTESIAN_POINT('Origin',(18.7,2.5,-0.5));
#8101=CARTESIAN_POINT('',(18.8,2.5,-0.16));
#8102=CARTESIAN_POINT('Origin',(18.8,2.5,-0.5));
#8103=CARTESIAN_POINT('',(20.3,2.5,-0.16));
#8104=CARTESIAN_POINT('',(18.7,2.5,-0.16));
#8105=CARTESIAN_POINT('Origin',(20.3,2.5,-0.5));
#8106=CARTESIAN_POINT('Origin',(18.7,2.5,4.5));
#8107=CARTESIAN_POINT('',(18.8,2.5,4.84));
#8108=CARTESIAN_POINT('Origin',(18.8,2.5,4.5));
#8109=CARTESIAN_POINT('',(20.3,2.5,4.84));
#8110=CARTESIAN_POINT('',(18.7,2.5,4.84));
#8111=CARTESIAN_POINT('Origin',(20.3,2.5,4.5));
#8112=CARTESIAN_POINT('Origin',(18.7,5.,-0.5));
#8113=CARTESIAN_POINT('',(18.8,5.,-0.16));
#8114=CARTESIAN_POINT('Origin',(18.8,5.,-0.5));
#8115=CARTESIAN_POINT('',(20.3,5.,-0.16));
#8116=CARTESIAN_POINT('',(18.7,5.,-0.16));
#8117=CARTESIAN_POINT('Origin',(20.3,5.,-0.5));
#8118=CARTESIAN_POINT('Origin',(18.7,5.,4.5));
#8119=CARTESIAN_POINT('',(18.8,5.,4.84));
#8120=CARTESIAN_POINT('Origin',(18.8,5.,4.5));
#8121=CARTESIAN_POINT('',(20.3,5.,4.84));
#8122=CARTESIAN_POINT('',(18.7,5.,4.84));
#8123=CARTESIAN_POINT('Origin',(20.3,5.,4.5));
#8124=CARTESIAN_POINT('Origin',(18.7,5.,9.5));
#8125=CARTESIAN_POINT('',(18.8,5.,9.84));
#8126=CARTESIAN_POINT('Origin',(18.8,5.,9.5));
#8127=CARTESIAN_POINT('',(20.3,5.,9.84));
#8128=CARTESIAN_POINT('',(18.7,5.,9.84));
#8129=CARTESIAN_POINT('Origin',(20.3,5.,9.5));
#8130=CARTESIAN_POINT('Origin',(20.3,7.5,-3.));
#8131=CARTESIAN_POINT('',(20.3,7.5,-3.));
#8132=CARTESIAN_POINT('',(18.8,7.5,-3.));
#8133=CARTESIAN_POINT('',(20.3,7.5,-3.));
#8134=CARTESIAN_POINT('',(18.8,7.5,12.));
#8135=CARTESIAN_POINT('',(18.8,7.5,-3.));
#8136=CARTESIAN_POINT('',(20.3,7.5,12.));
#8137=CARTESIAN_POINT('',(20.3,7.5,12.));
#8138=CARTESIAN_POINT('',(20.3,7.5,-3.));
#8139=CARTESIAN_POINT('Origin',(20.3,-7.5,-3.));
#8140=CARTESIAN_POINT('',(20.3,-7.5,-3.));
#8141=CARTESIAN_POINT('',(20.3,-7.5,-3.));
#8142=CARTESIAN_POINT('',(20.3,-7.5,12.));
#8143=CARTESIAN_POINT('',(20.3,-7.5,12.));
#8144=CARTESIAN_POINT('',(20.3,-7.5,-3.));
#8145=CARTESIAN_POINT('Origin',(18.8,-7.5,-3.));
#8146=CARTESIAN_POINT('',(18.8,-7.5,-3.));
#8147=CARTESIAN_POINT('',(18.8,-7.5,-3.));
#8148=CARTESIAN_POINT('',(18.8,-7.5,12.));
#8149=CARTESIAN_POINT('',(18.8,-7.5,12.));
#8150=CARTESIAN_POINT('',(18.8,-7.5,-3.));
#8151=CARTESIAN_POINT('Origin',(18.8,7.5,-3.));
#8152=CARTESIAN_POINT('',(18.8,7.5,-3.));
#8153=CARTESIAN_POINT('',(18.8,7.5,12.));
#8154=CARTESIAN_POINT('Origin',(19.55,0.,12.));
#8155=CARTESIAN_POINT('Origin',(19.55,0.,-3.));
#8156=CARTESIAN_POINT('',(0.,0.,0.));
#8157=CARTESIAN_POINT('Origin',(17.7,5.,4.5));
#8158=CARTESIAN_POINT('',(17.8,5.,4.925));
#8159=CARTESIAN_POINT('Origin',(17.8,5.,4.5));
#8160=CARTESIAN_POINT('',(18.8,5.,4.925));
#8161=CARTESIAN_POINT('',(17.7,5.,4.925));
#8162=CARTESIAN_POINT('Origin',(18.8,5.,4.5));
#8163=CARTESIAN_POINT('Origin',(17.7,5.,7.));
#8164=CARTESIAN_POINT('',(17.8,5.,7.425));
#8165=CARTESIAN_POINT('Origin',(17.8,5.,7.));
#8166=CARTESIAN_POINT('',(18.8,5.,7.425));
#8167=CARTESIAN_POINT('',(17.7,5.,7.425));
#8168=CARTESIAN_POINT('Origin',(18.8,5.,7.));
#8169=CARTESIAN_POINT('Origin',(18.8,5.5,3.5));
#8170=CARTESIAN_POINT('',(18.8,5.5,3.5));
#8171=CARTESIAN_POINT('',(17.8,5.5,3.5));
#8172=CARTESIAN_POINT('',(18.8,5.5,3.5));
#8173=CARTESIAN_POINT('',(17.8,5.5,8.5));
#8174=CARTESIAN_POINT('',(17.8,5.5,3.5));
#8175=CARTESIAN_POINT('',(18.8,5.5,8.5));
#8176=CARTESIAN_POINT('',(18.8,5.5,8.5));
#8177=CARTESIAN_POINT('',(18.8,5.5,3.5));
#8178=CARTESIAN_POINT('Origin',(18.8,4.5,3.5));
#8179=CARTESIAN_POINT('',(18.8,4.5,3.5));
#8180=CARTESIAN_POINT('',(18.8,4.5,3.5));
#8181=CARTESIAN_POINT('',(18.8,4.5,8.5));
#8182=CARTESIAN_POINT('',(18.8,4.5,8.5));
#8183=CARTESIAN_POINT('',(18.8,4.5,3.5));
#8184=CARTESIAN_POINT('Origin',(17.8,4.5,3.5));
#8185=CARTESIAN_POINT('',(17.8,4.5,3.5));
#8186=CARTESIAN_POINT('',(17.8,4.5,3.5));
#8187=CARTESIAN_POINT('',(17.8,4.5,8.5));
#8188=CARTESIAN_POINT('',(17.8,4.5,8.5));
#8189=CARTESIAN_POINT('',(17.8,4.5,3.5));
#8190=CARTESIAN_POINT('Origin',(17.8,5.5,3.5));
#8191=CARTESIAN_POINT('',(17.8,5.5,3.5));
#8192=CARTESIAN_POINT('',(17.8,5.5,8.5));
#8193=CARTESIAN_POINT('Origin',(18.3,5.,8.5));
#8194=CARTESIAN_POINT('Origin',(18.3,5.,3.5));
#8195=CARTESIAN_POINT('',(0.,0.,0.));
#8196=CARTESIAN_POINT('Origin',(0.,-1.445,0.));
#8197=CARTESIAN_POINT('',(-0.2942,-2.9458,3.60291088309151E-17));
#8198=CARTESIAN_POINT('Origin',(0.,-2.9458,0.));
#8199=CARTESIAN_POINT('',(-0.2942,0.,-3.60291088309151E-17));
#8200=CARTESIAN_POINT('',(-0.2942,-1.445,-3.60291088309151E-17));
#8201=CARTESIAN_POINT('Origin',(0.,0.,0.));
#8202=CARTESIAN_POINT('Origin',(0.,-2.97,0.));
#8203=CARTESIAN_POINT('',(-0.24,-3.,-2.93915231795365E-17));
#8204=CARTESIAN_POINT('Origin',(0.,-3.,0.));
#8205=CARTESIAN_POINT('',(-0.27,-2.97,-3.30654635769785E-17));
#8206=CARTESIAN_POINT('Origin',(0.,-3.,0.));
#8207=CARTESIAN_POINT('Origin',(0.,0.341586508806388,0.));
#8208=CARTESIAN_POINT('',(-0.475,0.4,-5.81707229594993E-17));
#8209=CARTESIAN_POINT('Origin',(0.,0.4,0.));
#8210=CARTESIAN_POINT('',(-0.577350269189626,0.340908044531739,-7.07050159149938E-17));
#8211=CARTESIAN_POINT('',(-0.576175134594813,0.341586508806388,-7.05611034329833E-17));
#8212=CARTESIAN_POINT('',(-0.288675134594813,0.340908044531739,0.5));
#8213=CARTESIAN_POINT('Ctrl Pts',(-0.288675134594813,0.340908044531739,
0.5));
#8214=CARTESIAN_POINT('Ctrl Pts',(-0.433012701893303,0.424241377863696,
0.249999999998124));
#8215=CARTESIAN_POINT('Ctrl Pts',(-0.577350269189626,0.340908044531739,
-7.07050159149938E-17));
#8216=CARTESIAN_POINT('',(0.288675134594813,0.340908044531739,0.5));
#8217=CARTESIAN_POINT('Ctrl Pts',(0.288675134594813,0.340908044531739,0.5));
#8218=CARTESIAN_POINT('Ctrl Pts',(-2.16648921025353E-12,0.424241377863696,
0.5));
#8219=CARTESIAN_POINT('Ctrl Pts',(-0.288675134594813,0.340908044531739,
0.5));
#8220=CARTESIAN_POINT('',(0.577350269189626,0.340908044531739,0.));
#8221=CARTESIAN_POINT('Ctrl Pts',(0.577350269189626,0.340908044531739,0.));
#8222=CARTESIAN_POINT('Ctrl Pts',(0.433012701891136,0.424241377863697,0.250000000001876));
#8223=CARTESIAN_POINT('Ctrl Pts',(0.288675134594813,0.340908044531739,0.5));
#8224=CARTESIAN_POINT('',(0.288675134594813,0.340908044531739,-0.5));
#8225=CARTESIAN_POINT('Ctrl Pts',(0.288675134594813,0.340908044531739,-0.5));
#8226=CARTESIAN_POINT('Ctrl Pts',(0.433012701893303,0.424241377863696,-0.249999999998124));
#8227=CARTESIAN_POINT('Ctrl Pts',(0.577350269189626,0.340908044531739,0.));
#8228=CARTESIAN_POINT('',(-0.288675134594813,0.340908044531739,-0.5));
#8229=CARTESIAN_POINT('Ctrl Pts',(-0.288675134594813,0.340908044531739,
-0.5));
#8230=CARTESIAN_POINT('Ctrl Pts',(2.16660023255599E-12,0.424241377863696,
-0.5));
#8231=CARTESIAN_POINT('Ctrl Pts',(0.288675134594813,0.340908044531739,-0.5));
#8232=CARTESIAN_POINT('Ctrl Pts',(-0.577350269189626,0.340908044531739,
-7.07050159149938E-17));
#8233=CARTESIAN_POINT('Ctrl Pts',(-0.433012701891136,0.424241377863697,
-0.250000000001876));
#8234=CARTESIAN_POINT('Ctrl Pts',(-0.288675134594813,0.340908044531739,
-0.5));
#8235=CARTESIAN_POINT('Origin',(0.288675134594813,0.,-0.5));
#8236=CARTESIAN_POINT('',(0.288675134594813,0.,-0.5));
#8237=CARTESIAN_POINT('',(0.288675134594813,0.,-0.5));
#8238=CARTESIAN_POINT('',(-0.288675134594813,0.,-0.5));
#8239=CARTESIAN_POINT('',(0.288675134594813,0.,-0.5));
#8240=CARTESIAN_POINT('',(-0.288675134594813,0.,-0.5));
#8241=CARTESIAN_POINT('Origin',(0.577350269189626,0.,0.));
#8242=CARTESIAN_POINT('',(0.577350269189626,0.,0.));
#8243=CARTESIAN_POINT('',(0.577350269189626,0.,0.));
#8244=CARTESIAN_POINT('',(0.577350269189626,0.,0.));
#8245=CARTESIAN_POINT('Origin',(0.288675134594813,0.,0.5));
#8246=CARTESIAN_POINT('',(0.288675134594813,0.,0.5));
#8247=CARTESIAN_POINT('',(0.288675134594813,0.,0.5));
#8248=CARTESIAN_POINT('',(0.288675134594813,0.,0.5));
#8249=CARTESIAN_POINT('Origin',(-0.288675134594813,0.,0.5));
#8250=CARTESIAN_POINT('',(-0.288675134594813,0.,0.5));
#8251=CARTESIAN_POINT('',(-0.288675134594813,0.,0.5));
#8252=CARTESIAN_POINT('',(-0.288675134594813,0.,0.5));
#8253=CARTESIAN_POINT('Origin',(-0.577350269189626,0.,-7.07050159149938E-17));
#8254=CARTESIAN_POINT('',(-0.577350269189626,0.,-7.07050159149938E-17));
#8255=CARTESIAN_POINT('',(-0.577350269189626,0.,-7.07050159149938E-17));
#8256=CARTESIAN_POINT('',(-0.577350269189626,0.,-7.07050159149938E-17));
#8257=CARTESIAN_POINT('Origin',(-0.288675134594813,0.,-0.5));
#8258=CARTESIAN_POINT('',(-0.288675134594813,0.,-0.5));
#8259=CARTESIAN_POINT('Origin',(0.,0.4,0.));
#8260=CARTESIAN_POINT('Origin',(0.,0.,0.));
#8261=CARTESIAN_POINT('',(0.,0.,0.));
#8262=CARTESIAN_POINT('Origin',(0.,0.0584134911936118,0.));
#8263=CARTESIAN_POINT('',(-0.288675134594813,0.0590919554682611,0.5));
#8264=CARTESIAN_POINT('',(0.288675134594813,0.0590919554682611,0.5));
#8265=CARTESIAN_POINT('Ctrl Pts',(-0.288675134594813,0.0590919554682611,
0.5));
#8266=CARTESIAN_POINT('Ctrl Pts',(2.1664336991023E-12,-0.0242413778636964,
0.5));
#8267=CARTESIAN_POINT('Ctrl Pts',(0.288675134594813,0.0590919554682611,
0.5));
#8268=CARTESIAN_POINT('',(-0.577350269189626,0.0590919554682611,-7.07050159149938E-17));
#8269=CARTESIAN_POINT('Ctrl Pts',(-0.577350269189626,0.0590919554682611,
-7.07050159149938E-17));
#8270=CARTESIAN_POINT('Ctrl Pts',(-0.433012701891136,-0.0242413778636963,
0.250000000001876));
#8271=CARTESIAN_POINT('Ctrl Pts',(-0.288675134594813,0.0590919554682611,
0.5));
#8272=CARTESIAN_POINT('',(-0.475,-4.16333634234434E-17,-5.81707229594993E-17));
#8273=CARTESIAN_POINT('',(-0.576175134594813,0.0584134911936118,-7.05611034329833E-17));
#8274=CARTESIAN_POINT('Origin',(0.,0.,0.));
#8275=CARTESIAN_POINT('',(-0.288675134594813,0.0590919554682611,-0.5));
#8276=CARTESIAN_POINT('Ctrl Pts',(-0.288675134594813,0.0590919554682611,
-0.5));
#8277=CARTESIAN_POINT('Ctrl Pts',(-0.433012701893303,-0.0242413778636963,
-0.249999999998124));
#8278=CARTESIAN_POINT('Ctrl Pts',(-0.577350269189626,0.0590919554682611,
-7.07050159149938E-17));
#8279=CARTESIAN_POINT('',(0.288675134594813,0.0590919554682611,-0.5));
#8280=CARTESIAN_POINT('Ctrl Pts',(0.288675134594813,0.0590919554682611,
-0.5));
#8281=CARTESIAN_POINT('Ctrl Pts',(-2.16648921025353E-12,-0.0242413778636962,
-0.5));
#8282=CARTESIAN_POINT('Ctrl Pts',(-0.288675134594813,0.0590919554682611,
-0.5));
#8283=CARTESIAN_POINT('',(0.577350269189626,0.0590919554682611,0.));
#8284=CARTESIAN_POINT('Ctrl Pts',(0.577350269189626,0.0590919554682611,
0.));
#8285=CARTESIAN_POINT('Ctrl Pts',(0.433012701891136,-0.0242413778636963,
-0.250000000001876));
#8286=CARTESIAN_POINT('Ctrl Pts',(0.288675134594813,0.0590919554682611,
-0.5));
#8287=CARTESIAN_POINT('Ctrl Pts',(0.288675134594813,0.0590919554682611,
0.5));
#8288=CARTESIAN_POINT('Ctrl Pts',(0.433012701893303,-0.0242413778636962,
0.249999999998124));
#8289=CARTESIAN_POINT('Ctrl Pts',(0.577350269189626,0.0590919554682611,
0.));
#8290=CARTESIAN_POINT('Origin',(0.,0.461586508806388,0.));
#8291=CARTESIAN_POINT('',(-0.475,0.52,-5.81707229594993E-17));
#8292=CARTESIAN_POINT('Origin',(0.,0.52,0.));
#8293=CARTESIAN_POINT('',(-0.577350269189626,0.460908044531739,-7.07050159149938E-17));
#8294=CARTESIAN_POINT('',(-0.576175134594813,0.461586508806388,-7.05611034329833E-17));
#8295=CARTESIAN_POINT('',(-0.288675134594813,0.460908044531739,0.5));
#8296=CARTESIAN_POINT('Ctrl Pts',(-0.288675134594813,0.460908044531739,
0.5));
#8297=CARTESIAN_POINT('Ctrl Pts',(-0.433012701893303,0.544241377863696,
0.249999999998124));
#8298=CARTESIAN_POINT('Ctrl Pts',(-0.577350269189626,0.460908044531739,
-7.07050159149938E-17));
#8299=CARTESIAN_POINT('',(0.288675134594813,0.460908044531739,0.5));
#8300=CARTESIAN_POINT('Ctrl Pts',(0.288675134594813,0.460908044531739,0.5));
#8301=CARTESIAN_POINT('Ctrl Pts',(-2.16676676600969E-12,0.544241377863697,
0.5));
#8302=CARTESIAN_POINT('Ctrl Pts',(-0.288675134594813,0.460908044531739,
0.5));
#8303=CARTESIAN_POINT('',(0.577350269189626,0.460908044531739,0.));
#8304=CARTESIAN_POINT('Ctrl Pts',(0.577350269189626,0.460908044531739,0.));
#8305=CARTESIAN_POINT('Ctrl Pts',(0.433012701891136,0.544241377863696,0.250000000001876));
#8306=CARTESIAN_POINT('Ctrl Pts',(0.288675134594813,0.460908044531739,0.5));
#8307=CARTESIAN_POINT('',(0.288675134594813,0.460908044531739,-0.5));
#8308=CARTESIAN_POINT('Ctrl Pts',(0.288675134594813,0.460908044531739,-0.5));
#8309=CARTESIAN_POINT('Ctrl Pts',(0.433012701893302,0.544241377863696,-0.249999999998124));
#8310=CARTESIAN_POINT('Ctrl Pts',(0.577350269189626,0.460908044531739,0.));
#8311=CARTESIAN_POINT('',(-0.288675134594813,0.460908044531739,-0.5));
#8312=CARTESIAN_POINT('Ctrl Pts',(-0.288675134594813,0.460908044531739,
-0.5));
#8313=CARTESIAN_POINT('Ctrl Pts',(2.16660023255599E-12,0.544241377863697,
-0.5));
#8314=CARTESIAN_POINT('Ctrl Pts',(0.288675134594813,0.460908044531739,-0.5));
#8315=CARTESIAN_POINT('Ctrl Pts',(-0.577350269189626,0.460908044531739,
-7.07050159149938E-17));
#8316=CARTESIAN_POINT('Ctrl Pts',(-0.433012701891136,0.544241377863696,
-0.250000000001876));
#8317=CARTESIAN_POINT('Ctrl Pts',(-0.288675134594813,0.460908044531739,
-0.5));
#8318=CARTESIAN_POINT('Origin',(0.288675134594813,0.,-0.5));
#8319=CARTESIAN_POINT('',(-0.288675134594813,0.,-0.5));
#8320=CARTESIAN_POINT('',(0.288675134594813,0.,-0.5));
#8321=CARTESIAN_POINT('Origin',(-0.288675134594813,0.,-0.5));
#8322=CARTESIAN_POINT('',(-0.577350269189626,0.,-7.07050159149938E-17));
#8323=CARTESIAN_POINT('Origin',(-0.577350269189626,0.,-7.07050159149938E-17));
#8324=CARTESIAN_POINT('',(-0.288675134594813,0.,0.5));
#8325=CARTESIAN_POINT('Origin',(0.,0.,0.));
#8326=CARTESIAN_POINT('',(-0.25175,0.52,3.08304831685346E-17));
#8327=CARTESIAN_POINT('Origin',(0.,0.52,0.));
#8328=CARTESIAN_POINT('',(-0.25175,0.,3.08304831685346E-17));
#8329=CARTESIAN_POINT('',(-0.25175,0.,3.08304831685346E-17));
#8330=CARTESIAN_POINT('Origin',(0.,0.,0.));
#8331=CARTESIAN_POINT('Origin',(-0.288675134594813,0.,0.5));
#8332=CARTESIAN_POINT('',(0.288675134594813,0.,0.5));
#8333=CARTESIAN_POINT('Origin',(0.577350269189626,0.,0.));
#8334=CARTESIAN_POINT('',(0.577350269189626,0.,0.));
#8335=CARTESIAN_POINT('Origin',(0.288675134594813,0.,0.5));
#8336=CARTESIAN_POINT('Origin',(0.,0.52,0.));
#8337=CARTESIAN_POINT('Origin',(0.,0.,0.));
#8338=CARTESIAN_POINT('',(0.,0.,0.));
#8339=CARTESIAN_POINT('Origin',(18.8,-2.5,2.));
#8340=CARTESIAN_POINT('',(19.8,-2.5,2.4));
#8341=CARTESIAN_POINT('Origin',(19.8,-2.5,2.));
#8342=CARTESIAN_POINT('',(18.8,-2.5,2.4));
#8343=CARTESIAN_POINT('',(18.8,-2.5,2.4));
#8344=CARTESIAN_POINT('Origin',(18.8,-2.5,2.));
#8345=CARTESIAN_POINT('Origin',(19.8,-2.5,2.));
#8346=CARTESIAN_POINT('Origin',(18.3,-2.5,2.));
#8347=CARTESIAN_POINT('',(18.8,-2.5,2.8));
#8348=CARTESIAN_POINT('Origin',(18.8,-2.5,2.));
#8349=CARTESIAN_POINT('',(18.3,-2.5,2.8));
#8350=CARTESIAN_POINT('',(18.3,-2.5,2.8));
#8351=CARTESIAN_POINT('Origin',(18.3,-2.5,2.));
#8352=CARTESIAN_POINT('Origin',(18.8,-2.5,2.));
#8353=CARTESIAN_POINT('Origin',(18.3,-2.5,2.));
#8354=CARTESIAN_POINT('',(0.,0.,0.));
#8355=CARTESIAN_POINT('Origin',(-8.04911692853238E-16,2.4,0.));
#8356=CARTESIAN_POINT('',(-0.3,2.91961524227066,-3.67394039744206E-17));
#8357=CARTESIAN_POINT('Origin',(0.,2.91961524227066,0.));
#8358=CARTESIAN_POINT('Origin',(0.,1.49980762113533,0.));
#8359=CARTESIAN_POINT('',(-0.3,0.0800000000000001,-3.67394039744206E-17));
#8360=CARTESIAN_POINT('Origin',(0.,0.08,0.));
#8361=CARTESIAN_POINT('',(-0.3,1.49980762113533,-3.67394039744206E-17));
#8362=CARTESIAN_POINT('Origin',(0.,0.04,0.));
#8363=CARTESIAN_POINT('',(-0.22,-6.93889390390723E-18,-2.69422295812418E-17));
#8364=CARTESIAN_POINT('Origin',(0.,0.,0.));
#8365=CARTESIAN_POINT('',(-0.26,0.04,-3.18408167778312E-17));
#8366=CARTESIAN_POINT('Origin',(0.,0.,0.));
#8367=CARTESIAN_POINT('',(0.,0.,0.));
#8368=CARTESIAN_POINT('Origin',(0.2,1.5,-0.4));
#8369=CARTESIAN_POINT('',(0.2,1.5,0.223606797749979));
#8370=CARTESIAN_POINT('',(0.2,1.5,-0.223606797749979));
#8371=CARTESIAN_POINT('Origin',(0.,1.5,0.));
#8372=CARTESIAN_POINT('',(0.2,1.5,-0.4));
#8373=CARTESIAN_POINT('Origin',(0.2,0.7,0.));
#8374=CARTESIAN_POINT('',(0.2,0.08,0.223606797749979));
#8375=CARTESIAN_POINT('',(0.2,1.49980762113533,0.223606797749979));
#8376=CARTESIAN_POINT('',(0.2,0.,0.0916515138991168));
#8377=CARTESIAN_POINT('Ctrl Pts',(0.2,0.,0.0916515138991168));
#8378=CARTESIAN_POINT('Ctrl Pts',(0.2,0.0232575029459984,0.147478749374482));
#8379=CARTESIAN_POINT('Ctrl Pts',(0.2,0.08,0.223606797749979));
#8380=CARTESIAN_POINT('',(0.2,0.,-0.0916515138991168));
#8381=CARTESIAN_POINT('',(0.2,0.,0.));
#8382=CARTESIAN_POINT('',(0.2,0.08,-0.223606797749979));
#8383=CARTESIAN_POINT('Ctrl Pts',(0.2,0.08,-0.223606797749979));
#8384=CARTESIAN_POINT('Ctrl Pts',(0.2,0.0232575029459984,-0.147478749374482));
#8385=CARTESIAN_POINT('Ctrl Pts',(0.2,0.,-0.0916515138991168));
#8386=CARTESIAN_POINT('',(0.2,1.49980762113533,-0.223606797749979));
#8387=CARTESIAN_POINT('Origin',(0.,1.49980762113533,0.));
#8388=CARTESIAN_POINT('',(-0.2,0.08,-0.223606797749979));
#8389=CARTESIAN_POINT('Origin',(0.,0.08,0.));
#8390=CARTESIAN_POINT('',(-0.2,1.5,-0.223606797749979));
#8391=CARTESIAN_POINT('',(-0.2,1.49980762113533,-0.223606797749979));
#8392=CARTESIAN_POINT('',(-0.3,1.5,-3.67394039744206E-17));
#8393=CARTESIAN_POINT('Origin',(0.,1.5,0.));
#8394=CARTESIAN_POINT('',(-0.3,2.91961524227066,-3.67394039744206E-17));
#8395=CARTESIAN_POINT('',(-0.3,1.49980762113533,-3.67394039744206E-17));
#8396=CARTESIAN_POINT('Origin',(0.,2.91961524227066,0.));
#8397=CARTESIAN_POINT('',(-0.2,1.5,0.223606797749979));
#8398=CARTESIAN_POINT('Origin',(0.,1.5,0.));
#8399=CARTESIAN_POINT('',(-0.2,0.08,0.223606797749979));
#8400=CARTESIAN_POINT('',(-0.2,1.49980762113533,0.223606797749979));
#8401=CARTESIAN_POINT('Origin',(0.,0.08,0.));
#8402=CARTESIAN_POINT('Origin',(0.,0.04,0.));
#8403=CARTESIAN_POINT('',(-0.2,0.,-0.0916515138991168));
#8404=CARTESIAN_POINT('Origin',(0.,0.,0.));
#8405=CARTESIAN_POINT('Ctrl Pts',(-0.2,0.,-0.0916515138991168));
#8406=CARTESIAN_POINT('Ctrl Pts',(-0.2,0.0232575029459984,-0.147478749374482));
#8407=CARTESIAN_POINT('Ctrl Pts',(-0.2,0.08,-0.223606797749979));
#8408=CARTESIAN_POINT('Origin',(-0.2,0.7,0.));
#8409=CARTESIAN_POINT('',(-0.2,1.5,-0.4));
#8410=CARTESIAN_POINT('',(-0.2,0.,0.0916515138991168));
#8411=CARTESIAN_POINT('',(-0.2,0.,0.));
#8412=CARTESIAN_POINT('Ctrl Pts',(-0.2,0.08,0.223606797749979));
#8413=CARTESIAN_POINT('Ctrl Pts',(-0.2,0.0232575029459984,0.147478749374482));
#8414=CARTESIAN_POINT('Ctrl Pts',(-0.2,0.,0.0916515138991168));
#8415=CARTESIAN_POINT('Origin',(-0.4,1.5,-0.4));
#8416=CARTESIAN_POINT('Origin',(0.,0.,0.));
#8417=CARTESIAN_POINT('Origin',(0.,0.,0.));
#8418=CARTESIAN_POINT('Origin',(-8.04911692853238E-16,2.4,0.));
#8419=CARTESIAN_POINT('Origin',(0.,0.04,0.));
#8420=CARTESIAN_POINT('',(0.,0.,0.));
#8421=CARTESIAN_POINT('Origin',(0.173205080756888,-0.8,-0.3));
#8422=CARTESIAN_POINT('',(0.346410161513775,-0.8,0.));
#8423=CARTESIAN_POINT('',(0.173205080756888,-0.8,-0.3));
#8424=CARTESIAN_POINT('',(0.346410161513775,-0.8,0.));
#8425=CARTESIAN_POINT('',(0.173205080756888,-1.28,-0.3));
#8426=CARTESIAN_POINT('',(0.173205080756888,-0.8,-0.3));
#8427=CARTESIAN_POINT('',(0.346410161513775,-1.28,0.));
#8428=CARTESIAN_POINT('',(0.346410161513775,-1.28,0.));
#8429=CARTESIAN_POINT('',(0.346410161513775,-0.8,0.));
#8430=CARTESIAN_POINT('Origin',(-0.173205080756888,-0.8,-0.3));
#8431=CARTESIAN_POINT('',(-0.173205080756888,-0.8,-0.3));
#8432=CARTESIAN_POINT('',(0.173205080756888,-0.8,-0.3));
#8433=CARTESIAN_POINT('',(-0.173205080756888,-1.28,-0.3));
#8434=CARTESIAN_POINT('',(-0.173205080756888,-0.8,-0.3));
#8435=CARTESIAN_POINT('',(0.173205080756888,-1.28,-0.3));
#8436=CARTESIAN_POINT('Origin',(-0.346410161513775,-0.8,-5.55111512312578E-17));
#8437=CARTESIAN_POINT('',(-0.346410161513775,-0.8,-4.24230095489963E-17));
#8438=CARTESIAN_POINT('',(-0.173205080756888,-0.8,-0.3));
#8439=CARTESIAN_POINT('',(-0.346410161513775,-1.28,-5.55111512312578E-17));
#8440=CARTESIAN_POINT('',(-0.346410161513775,-0.8,-4.24230095489963E-17));
#8441=CARTESIAN_POINT('',(-0.173205080756888,-1.28,-0.3));
#8442=CARTESIAN_POINT('Origin',(-0.173205080756888,-0.8,0.3));
#8443=CARTESIAN_POINT('',(-0.173205080756888,-0.8,0.3));
#8444=CARTESIAN_POINT('',(-0.346410161513775,-0.8,-4.24230095489963E-17));
#8445=CARTESIAN_POINT('',(-0.173205080756888,-1.28,0.3));
#8446=CARTESIAN_POINT('',(-0.173205080756888,-0.8,0.3));
#8447=CARTESIAN_POINT('',(-0.346410161513775,-1.28,-4.24230095489963E-17));
#8448=CARTESIAN_POINT('Origin',(0.173205080756888,-0.8,0.3));
#8449=CARTESIAN_POINT('',(0.173205080756888,-0.8,0.3));
#8450=CARTESIAN_POINT('',(-0.173205080756888,-0.8,0.3));
#8451=CARTESIAN_POINT('',(0.173205080756888,-1.28,0.3));
#8452=CARTESIAN_POINT('',(0.173205080756888,-0.8,0.3));
#8453=CARTESIAN_POINT('',(-0.173205080756888,-1.28,0.3));
#8454=CARTESIAN_POINT('Origin',(0.346410161513775,-0.8,0.));
#8455=CARTESIAN_POINT('',(0.173205080756888,-0.8,0.3));
#8456=CARTESIAN_POINT('',(0.173205080756888,-1.28,0.3));
#8457=CARTESIAN_POINT('Origin',(0.,-0.8,-5.55111512312578E-17));
#8458=CARTESIAN_POINT('Origin',(0.,-1.28,-5.55111512312578E-17));
#8459=CARTESIAN_POINT('Origin',(0.,-2.5,0.));
#8460=CARTESIAN_POINT('',(-0.3933,-2.5,4.81653586104654E-17));
#8461=CARTESIAN_POINT('Origin',(0.,-2.5,0.));
#8462=CARTESIAN_POINT('Origin',(0.6,0.8,0.));
#8463=CARTESIAN_POINT('',(-0.6,0.8,-7.34788079488412E-17));
#8464=CARTESIAN_POINT('Origin',(0.,0.8,0.));
#8465=CARTESIAN_POINT('Origin',(0.,0.775,0.));
#8466=CARTESIAN_POINT('',(-0.65,0.75,-7.9602041944578E-17));
#8467=CARTESIAN_POINT('Origin',(0.,0.75,0.));
#8468=CARTESIAN_POINT('',(-0.625,0.775,-7.65404249467096E-17));
#8469=CARTESIAN_POINT('Origin',(0.,0.39,0.));
#8470=CARTESIAN_POINT('',(-0.65,0.0299999999999998,-7.9602041944578E-17));
#8471=CARTESIAN_POINT('Origin',(0.,0.0299999999999998,0.));
#8472=CARTESIAN_POINT('',(-0.65,0.39,-7.9602041944578E-17));
#8473=CARTESIAN_POINT('Origin',(0.,0.0150000000000001,0.));
#8474=CARTESIAN_POINT('',(-0.62,5.89805981832114E-17,-7.59281015471359E-17));
#8475=CARTESIAN_POINT('Origin',(0.,0.,0.));
#8476=CARTESIAN_POINT('',(-0.635,0.0150000000000001,-7.77650717458569E-17));
#8477=CARTESIAN_POINT('Origin',(0.42,0.,0.));
#8478=CARTESIAN_POINT('',(-0.42,-3.46944695195361E-18,-5.14351655641888E-17));
#8479=CARTESIAN_POINT('Origin',(0.,0.,0.));
#8480=CARTESIAN_POINT('Origin',(0.,-0.02,0.));
#8481=CARTESIAN_POINT('',(-0.3933,-0.0534000000000001,4.81653586104654E-17));
#8482=CARTESIAN_POINT('Origin',(0.,-0.0534000000000001,0.));
#8483=CARTESIAN_POINT('',(-0.41,-0.02,-5.02105187650415E-17));
#8484=CARTESIAN_POINT('Origin',(0.,-1.48,0.));
#8485=CARTESIAN_POINT('',(-0.3933,-1.48,-4.81653586104654E-17));
#8486=CARTESIAN_POINT('',(0.,0.,0.));
#8487=CARTESIAN_POINT('',(0.,0.,0.));
#8488=CARTESIAN_POINT('Origin',(0.435778713738291,-0.4,7.48097349045873));
#8489=CARTESIAN_POINT('',(0.160778713738291,-0.3,7.48097349045873));
#8490=CARTESIAN_POINT('Origin',(0.435778713738291,-0.3,7.48097349045873));
#8491=CARTESIAN_POINT('',(0.160778713738291,0.3,7.48097349045873));
#8492=CARTESIAN_POINT('',(0.160778713738291,-0.4,7.48097349045873));
#8493=CARTESIAN_POINT('Origin',(0.435778713738291,0.3,7.48097349045873));
#8494=CARTESIAN_POINT('Origin',(0.,-0.6,2.5));
#8495=CARTESIAN_POINT('',(-0.31,-0.48,2.5));
#8496=CARTESIAN_POINT('Origin',(0.,-0.48,2.5));
#8497=CARTESIAN_POINT('',(-0.31,0.48,2.5));
#8498=CARTESIAN_POINT('',(-0.31,-0.6,2.5));
#8499=CARTESIAN_POINT('Origin',(0.,0.48,2.5));
#8500=CARTESIAN_POINT('Origin',(0.435778713738291,-0.3,7.48097349045873));
#8501=CARTESIAN_POINT('',(0.784189430553042,0.3,6.87384090822596));
#8502=CARTESIAN_POINT('',(0.784189430553042,-0.3,6.87384090822596));
#8503=CARTESIAN_POINT('',(0.784189430553042,-0.3,6.87384090822596));
#8504=CARTESIAN_POINT('',(-0.0127663279203548,0.3,6.94356550242408));
#8505=CARTESIAN_POINT('Origin',(0.435778713738291,0.3,7.48097349045873));
#8506=CARTESIAN_POINT('',(-0.0127663279203548,-0.3,6.94356550242408));
#8507=CARTESIAN_POINT('',(-0.0127663279203548,-0.3,6.94356550242408));
#8508=CARTESIAN_POINT('Origin',(0.435778713738291,-0.3,7.48097349045873));
#8509=CARTESIAN_POINT('Origin',(0.217889356869145,-0.3,4.99048674522937));
#8510=CARTESIAN_POINT('',(-0.359500646154049,-0.3,2.98037410985067));
#8511=CARTESIAN_POINT('',(-0.398477879236698,-0.3,2.53486229709906));
#8512=CARTESIAN_POINT('',(0.437455112319348,-0.3,2.91064951565254));
#8513=CARTESIAN_POINT('Origin',(0.,-0.3,2.5));
#8514=CARTESIAN_POINT('',(0.834256592974989,-0.3,7.44611119335967));
#8515=CARTESIAN_POINT('Origin',(-0.398477879236698,-0.3,2.53486229709906));
#8516=CARTESIAN_POINT('',(-0.359500646154049,0.3,2.98037410985067));
#8517=CARTESIAN_POINT('',(-0.398477879236698,0.3,2.53486229709906));
#8518=CARTESIAN_POINT('',(-0.359500646154049,-0.48,2.98037410985067));
#8519=CARTESIAN_POINT('Origin',(0.217889356869145,0.3,4.99048674522937));
#8520=CARTESIAN_POINT('',(0.437455112319348,0.3,2.91064951565254));
#8521=CARTESIAN_POINT('',(0.834256592974989,0.3,7.44611119335967));
#8522=CARTESIAN_POINT('Origin',(0.,0.3,2.5));
#8523=CARTESIAN_POINT('Origin',(0.834256592974989,-0.3,7.44611119335967));
#8524=CARTESIAN_POINT('',(0.437455112319348,-0.48,2.91064951565254));
#8525=CARTESIAN_POINT('Origin',(2.49048674522936,-1.,2.28211064313085));
#8526=CARTESIAN_POINT('',(2.18048674522936,-0.9,2.28211064313085));
#8527=CARTESIAN_POINT('Origin',(2.49048674522936,-0.9,2.28211064313085));
#8528=CARTESIAN_POINT('',(2.18048674522936,-0.5,2.28211064313085));
#8529=CARTESIAN_POINT('',(2.18048674522936,-1.,2.28211064313085));
#8530=CARTESIAN_POINT('Origin',(2.49048674522936,-0.5,2.28211064313085));
#8531=CARTESIAN_POINT('Origin',(2.49048674522936,-1.,2.28211064313085));
#8532=CARTESIAN_POINT('',(2.18048674522936,0.5,2.28211064313085));
#8533=CARTESIAN_POINT('Origin',(2.49048674522936,0.5,2.28211064313085));
#8534=CARTESIAN_POINT('',(2.18048674522936,0.9,2.28211064313085));
#8535=CARTESIAN_POINT('',(2.18048674522936,-1.,2.28211064313085));
#8536=CARTESIAN_POINT('Origin',(2.49048674522936,0.9,2.28211064313085));
#8537=CARTESIAN_POINT('Origin',(1.66363611114492,-0.9,3.15750657007714));
#8538=CARTESIAN_POINT('',(1.52418692274867,-0.5,1.56359505313035));
#8539=CARTESIAN_POINT('',(1.66363611114492,-0.5,3.15750657007714));
#8540=CARTESIAN_POINT('',(1.62877381404586,-0.5,2.75902869084045));
#8541=CARTESIAN_POINT('',(1.52418692274867,0.5,1.56359505313035));
#8542=CARTESIAN_POINT('',(1.52418692274867,-0.9,1.56359505313035));
#8543=CARTESIAN_POINT('',(1.66363611114492,0.5,3.15750657007714));
#8544=CARTESIAN_POINT('',(1.62877381404586,0.5,2.75902869084045));
#8545=CARTESIAN_POINT('',(1.66363611114492,-0.9,3.15750657007714));
#8546=CARTESIAN_POINT('Origin',(2.29124780561101,0.9,2.29954179168039));
#8547=CARTESIAN_POINT('',(1.3647777017174,0.9,3.18365329290144));
#8548=CARTESIAN_POINT('',(3.35716709790089,0.9,3.00934180740612));
#8549=CARTESIAN_POINT('',(3.35716709790089,0.9,3.00934180740612));
#8550=CARTESIAN_POINT('',(3.21771790950463,0.9,1.41543029045933));
#8551=CARTESIAN_POINT('',(3.21771790950463,0.9,1.41543029045933));
#8552=CARTESIAN_POINT('',(1.22532851332114,0.9,1.58974177595465));
#8553=CARTESIAN_POINT('',(1.22532851332114,0.9,1.58974177595465));
#8554=CARTESIAN_POINT('',(1.3647777017174,0.9,3.18365329290144));
#8555=CARTESIAN_POINT('Origin',(3.35716709790089,0.5,3.00934180740612));
#8556=CARTESIAN_POINT('',(3.21771790950463,0.5,1.41543029045933));
#8557=CARTESIAN_POINT('',(3.35716709790089,0.5,3.00934180740612));
#8558=CARTESIAN_POINT('',(3.21771790950463,0.5,1.41543029045933));
#8559=CARTESIAN_POINT('',(3.21771790950463,0.5,1.41543029045933));
#8560=CARTESIAN_POINT('',(3.35716709790089,0.5,3.00934180740612));
#8561=CARTESIAN_POINT('Origin',(2.29124780561101,0.5,2.29954179168039));
#8562=CARTESIAN_POINT('',(1.22532851332114,0.5,1.58974177595465));
#8563=CARTESIAN_POINT('',(3.35716709790089,0.5,3.00934180740612));
#8564=CARTESIAN_POINT('Origin',(0.747146023568809,-0.3,2.43463319293926));
#8565=CARTESIAN_POINT('',(1.26019081042021,-0.3,1.98821965519135));
#8566=CARTESIAN_POINT('',(1.32991540461833,-0.3,2.78517541366474));
#8567=CARTESIAN_POINT('',(1.26019081042021,-0.3,1.98821965519135));
#8568=CARTESIAN_POINT('',(0.480374109850668,-0.3,2.85950064615405));
#8569=CARTESIAN_POINT('',(0.0348622970990633,-0.3,2.8984778792367));
#8570=CARTESIAN_POINT('',(0.410649515652541,-0.3,2.06254488768065));
#8571=CARTESIAN_POINT('Origin',(0.,-0.3,2.5));
#8572=CARTESIAN_POINT('',(1.45942975003856,-0.3,1.97078850664181));
#8573=CARTESIAN_POINT('Origin',(0.0348622970990633,-0.3,2.8984778792367));
#8574=CARTESIAN_POINT('',(1.32991540461833,0.3,2.78517541366474));
#8575=CARTESIAN_POINT('',(1.32991540461833,-0.6,2.78517541366474));
#8576=CARTESIAN_POINT('',(0.480374109850668,0.3,2.85950064615405));
#8577=CARTESIAN_POINT('',(0.0348622970990633,0.3,2.8984778792367));
#8578=CARTESIAN_POINT('',(0.480374109850668,-0.48,2.85950064615405));
#8579=CARTESIAN_POINT('Origin',(0.747146023568809,0.3,2.43463319293926));
#8580=CARTESIAN_POINT('',(1.26019081042021,0.3,1.98821965519135));
#8581=CARTESIAN_POINT('',(1.26019081042021,0.3,1.98821965519135));
#8582=CARTESIAN_POINT('',(0.410649515652541,0.3,2.06254488768065));
#8583=CARTESIAN_POINT('',(1.45942975003856,0.3,1.97078850664181));
#8584=CARTESIAN_POINT('Origin',(0.,0.3,2.5));
#8585=CARTESIAN_POINT('Origin',(1.45942975003856,-0.3,1.97078850664181));
#8586=CARTESIAN_POINT('',(1.26019081042021,-0.6,1.98821965519135));
#8587=CARTESIAN_POINT('',(0.410649515652541,-0.48,2.06254488768065));
#8588=CARTESIAN_POINT('Origin',(0.,-0.48,2.5));
#8589=CARTESIAN_POINT('',(-0.6,0.48,2.5));
#8590=CARTESIAN_POINT('Origin',(0.,0.48,2.5));
#8591=CARTESIAN_POINT('',(-0.6,-0.48,2.5));
#8592=CARTESIAN_POINT('',(-0.6,-0.48,2.5));
#8593=CARTESIAN_POINT('Origin',(0.,-0.48,2.5));
#8594=CARTESIAN_POINT('Origin',(0.,0.48,2.5));
#8595=CARTESIAN_POINT('Origin',(0.,-0.48,2.5));
#8596=CARTESIAN_POINT('Origin',(3.21771790950463,-0.9,1.41543029045933));
#8597=CARTESIAN_POINT('',(3.21771790950463,-0.5,1.41543029045933));
#8598=CARTESIAN_POINT('',(1.22532851332114,-0.5,1.58974177595465));
#8599=CARTESIAN_POINT('',(3.21771790950463,-0.9,1.41543029045933));
#8600=CARTESIAN_POINT('',(3.21771790950463,-0.9,1.41543029045933));
#8601=CARTESIAN_POINT('',(1.22532851332114,-0.9,1.58974177595465));
#8602=CARTESIAN_POINT('',(1.22532851332114,-0.9,1.58974177595465));
#8603=CARTESIAN_POINT('',(1.22532851332114,-0.9,1.58974177595465));
#8604=CARTESIAN_POINT('Origin',(2.29124780561101,-0.5,2.29954179168039));
#8605=CARTESIAN_POINT('',(3.35716709790089,-0.5,3.00934180740612));
#8606=CARTESIAN_POINT('',(3.35716709790089,-0.5,3.00934180740612));
#8607=CARTESIAN_POINT('',(3.21771790950463,-0.5,1.41543029045933));
#8608=CARTESIAN_POINT('Origin',(1.22532851332114,-0.9,1.58974177595465));
#8609=CARTESIAN_POINT('',(1.3647777017174,-0.9,3.18365329290144));
#8610=CARTESIAN_POINT('',(1.3647777017174,-0.9,3.18365329290144));
#8611=CARTESIAN_POINT('',(1.3647777017174,-0.9,3.18365329290144));
#8612=CARTESIAN_POINT('Origin',(3.35716709790089,-0.9,3.00934180740612));
#8613=CARTESIAN_POINT('',(3.35716709790089,-0.9,3.00934180740612));
#8614=CARTESIAN_POINT('',(3.21771790950463,-0.9,1.41543029045933));
#8615=CARTESIAN_POINT('',(3.35716709790089,-0.9,3.00934180740612));
#8616=CARTESIAN_POINT('Origin',(1.3647777017174,-0.9,3.18365329290144));
#8617=CARTESIAN_POINT('',(3.35716709790089,-0.9,3.00934180740612));
#8618=CARTESIAN_POINT('Origin',(2.29124780561101,-0.9,2.29954179168039));
#8619=CARTESIAN_POINT('',(0.,0.,0.));
#8620=CARTESIAN_POINT('Origin',(0.,-7.7,10.03));
#8621=CARTESIAN_POINT('',(-0.21,-7.7,10.03));
#8622=CARTESIAN_POINT('Origin',(0.,-7.7,10.03));
#8623=CARTESIAN_POINT('',(-0.21,-6.5,10.03));
#8624=CARTESIAN_POINT('',(-0.21,-7.7,10.03));
#8625=CARTESIAN_POINT('Origin',(0.,-6.5,10.03));
#8626=CARTESIAN_POINT('Origin',(0.,-7.7,10.03));
#8627=CARTESIAN_POINT('Origin',(0.,-9.5,10.03));
#8628=CARTESIAN_POINT('',(-0.7,-6.5,10.03));
#8629=CARTESIAN_POINT('Origin',(0.,-6.5,10.03));
#8630=CARTESIAN_POINT('',(-0.7,-9.5,10.03));
#8631=CARTESIAN_POINT('',(-0.7,-9.5,10.03));
#8632=CARTESIAN_POINT('Origin',(0.,-9.5,10.03));
#8633=CARTESIAN_POINT('Origin',(0.,-6.5,10.03));
#8634=CARTESIAN_POINT('Origin',(0.,-9.5,10.03));
#8635=CARTESIAN_POINT('',(0.,0.,0.));
#8636=CARTESIAN_POINT('Origin',(0.115470053837925,-0.5,-0.2));
#8637=CARTESIAN_POINT('',(0.23094010767585,-0.5,0.));
#8638=CARTESIAN_POINT('',(0.115470053837925,-0.5,-0.2));
#8639=CARTESIAN_POINT('',(0.23094010767585,-0.5,0.));
#8640=CARTESIAN_POINT('',(0.115470053837925,-0.8,-0.2));
#8641=CARTESIAN_POINT('',(0.115470053837925,-0.5,-0.2));
#8642=CARTESIAN_POINT('',(0.23094010767585,-0.8,0.));
#8643=CARTESIAN_POINT('',(0.23094010767585,-0.8,0.));
#8644=CARTESIAN_POINT('',(0.23094010767585,-0.5,0.));
#8645=CARTESIAN_POINT('Origin',(-0.115470053837925,-0.5,-0.2));
#8646=CARTESIAN_POINT('',(-0.115470053837925,-0.5,-0.2));
#8647=CARTESIAN_POINT('',(0.115470053837925,-0.5,-0.2));
#8648=CARTESIAN_POINT('',(-0.115470053837925,-0.8,-0.2));
#8649=CARTESIAN_POINT('',(-0.115470053837925,-0.5,-0.2));
#8650=CARTESIAN_POINT('',(0.115470053837925,-0.8,-0.2));
#8651=CARTESIAN_POINT('Origin',(-0.23094010767585,-0.5,-2.77555756156289E-17));
#8652=CARTESIAN_POINT('',(-0.23094010767585,-0.5,-2.82820063659975E-17));
#8653=CARTESIAN_POINT('',(-0.115470053837925,-0.5,-0.2));
#8654=CARTESIAN_POINT('',(-0.23094010767585,-0.8,-2.77555756156289E-17));
#8655=CARTESIAN_POINT('',(-0.23094010767585,-0.5,-2.82820063659975E-17));
#8656=CARTESIAN_POINT('',(-0.115470053837925,-0.8,-0.2));
#8657=CARTESIAN_POINT('Origin',(-0.115470053837925,-0.5,0.2));
#8658=CARTESIAN_POINT('',(-0.115470053837925,-0.5,0.2));
#8659=CARTESIAN_POINT('',(-0.23094010767585,-0.5,-2.82820063659975E-17));
#8660=CARTESIAN_POINT('',(-0.115470053837925,-0.8,0.2));
#8661=CARTESIAN_POINT('',(-0.115470053837925,-0.5,0.2));
#8662=CARTESIAN_POINT('',(-0.23094010767585,-0.8,-2.82820063659975E-17));
#8663=CARTESIAN_POINT('Origin',(0.115470053837925,-0.5,0.2));
#8664=CARTESIAN_POINT('',(0.115470053837925,-0.5,0.2));
#8665=CARTESIAN_POINT('',(-0.115470053837925,-0.5,0.2));
#8666=CARTESIAN_POINT('',(0.115470053837925,-0.8,0.2));
#8667=CARTESIAN_POINT('',(0.115470053837925,-0.5,0.2));
#8668=CARTESIAN_POINT('',(-0.115470053837925,-0.8,0.2));
#8669=CARTESIAN_POINT('Origin',(0.23094010767585,-0.5,0.));
#8670=CARTESIAN_POINT('',(0.115470053837925,-0.5,0.2));
#8671=CARTESIAN_POINT('',(0.115470053837925,-0.8,0.2));
#8672=CARTESIAN_POINT('Origin',(0.,-0.5,0.));
#8673=CARTESIAN_POINT('Origin',(0.,-0.8,0.));
#8674=CARTESIAN_POINT('Origin',(0.,-1.4,0.));
#8675=CARTESIAN_POINT('',(-0.24505,-1.4,3.00099698131059E-17));
#8676=CARTESIAN_POINT('Origin',(0.,-1.4,0.));
#8677=CARTESIAN_POINT('Origin',(0.375,0.5,0.));
#8678=CARTESIAN_POINT('',(-0.375,0.5,-4.59242549680257E-17));
#8679=CARTESIAN_POINT('Origin',(0.,0.5,0.));
#8680=CARTESIAN_POINT('Origin',(0.,0.475,0.));
#8681=CARTESIAN_POINT('',(-0.425,0.45,-5.20474889637625E-17));
#8682=CARTESIAN_POINT('Origin',(0.,0.45,0.));
#8683=CARTESIAN_POINT('',(-0.4,0.475,-4.89858719658941E-17));
#8684=CARTESIAN_POINT('Origin',(0.,0.24,0.));
#8685=CARTESIAN_POINT('',(-0.425,0.0299999999999998,-5.20474889637625E-17));
#8686=CARTESIAN_POINT('Origin',(0.,0.0299999999999998,0.));
#8687=CARTESIAN_POINT('',(-0.425,0.24,-5.20474889637625E-17));
#8688=CARTESIAN_POINT('Origin',(0.,0.0150000000000001,0.));
#8689=CARTESIAN_POINT('',(-0.395,4.85722573273506E-17,-4.83735485663204E-17));
#8690=CARTESIAN_POINT('Origin',(0.,0.,0.));
#8691=CARTESIAN_POINT('',(-0.41,0.0150000000000001,-5.02105187650415E-17));
#8692=CARTESIAN_POINT('Origin',(0.27,0.,0.));
#8693=CARTESIAN_POINT('',(-0.27,0.,-3.30654635769785E-17));
#8694=CARTESIAN_POINT('Origin',(0.,0.,0.));
#8695=CARTESIAN_POINT('Origin',(0.,-0.02,0.));
#8696=CARTESIAN_POINT('',(-0.24505,-0.0498999999999999,3.00099698131059E-17));
#8697=CARTESIAN_POINT('Origin',(0.,-0.0498999999999999,0.));
#8698=CARTESIAN_POINT('',(-0.26,-0.02,-3.18408167778312E-17));
#8699=CARTESIAN_POINT('Origin',(0.,-0.995,0.));
#8700=CARTESIAN_POINT('',(-0.24505,-0.995,-3.00099698131059E-17));
#8701=CARTESIAN_POINT('',(0.,0.,0.));
#8702=CARTESIAN_POINT('',(0.,0.,0.));
#8703=CARTESIAN_POINT('Origin',(2.49048674522936,-0.6,2.28211064313085));
#8704=CARTESIAN_POINT('',(2.18048674522936,-0.48,2.28211064313085));
#8705=CARTESIAN_POINT('Origin',(2.49048674522936,-0.48,2.28211064313085));
#8706=CARTESIAN_POINT('',(2.18048674522936,0.48,2.28211064313085));
#8707=CARTESIAN_POINT('',(2.18048674522936,-0.6,2.28211064313085));
#8708=CARTESIAN_POINT('Origin',(2.49048674522936,0.48,2.28211064313085));
#8709=CARTESIAN_POINT('Origin',(5.98369790806552,-0.6,2.5));
#8710=CARTESIAN_POINT('',(5.67369790806552,-0.48,2.5));
#8711=CARTESIAN_POINT('Origin',(5.98369790806552,-0.48,2.5));
#8712=CARTESIAN_POINT('',(5.67369790806552,0.48,2.5));
#8713=CARTESIAN_POINT('',(5.67369790806552,-0.6,2.5));
#8714=CARTESIAN_POINT('Origin',(5.98369790806552,0.48,2.5));
#8715=CARTESIAN_POINT('Origin',(5.98369790806552,-0.48,2.5));
#8716=CARTESIAN_POINT('',(5.56225339914413,0.48,2.07293498633112));
#8717=CARTESIAN_POINT('',(5.56225339914413,-0.48,2.07293498633112));
#8718=CARTESIAN_POINT('',(5.56225339914413,-0.48,2.07293498633112));
#8719=CARTESIAN_POINT('',(5.51245011757404,0.48,2.87138325212224));
#8720=CARTESIAN_POINT('Origin',(5.98369790806552,0.48,2.5));
#8721=CARTESIAN_POINT('',(5.51245011757404,-0.48,2.87138325212224));
#8722=CARTESIAN_POINT('',(5.51245011757404,-0.48,2.87138325212224));
#8723=CARTESIAN_POINT('Origin',(5.98369790806552,-0.48,2.5));
#8724=CARTESIAN_POINT('Origin',(6.00859954885057,-0.48,2.10077586710444));
#8725=CARTESIAN_POINT('',(2.96173453572085,-0.48,1.91072739100861));
#8726=CARTESIAN_POINT('',(6.00859954885057,-0.48,2.10077586710444));
#8727=CARTESIAN_POINT('',(2.96173453572085,0.48,1.91072739100861));
#8728=CARTESIAN_POINT('',(2.96173453572085,-0.48,1.91072739100861));
#8729=CARTESIAN_POINT('',(6.00859954885057,0.48,2.10077586710444));
#8730=CARTESIAN_POINT('Origin',(2.49048674522936,-0.48,2.28211064313085));
#8731=CARTESIAN_POINT('',(2.91193125415076,-0.48,2.70917565679974));
#8732=CARTESIAN_POINT('',(2.46558510444432,-0.48,2.68133477602642));
#8733=CARTESIAN_POINT('Origin',(2.49048674522936,-0.48,2.28211064313085));
#8734=CARTESIAN_POINT('Origin',(2.46558510444432,-0.48,2.68133477602642));
#8735=CARTESIAN_POINT('',(2.91193125415076,0.48,2.70917565679974));
#8736=CARTESIAN_POINT('',(2.46558510444432,0.48,2.68133477602642));
#8737=CARTESIAN_POINT('',(2.91193125415076,-0.48,2.70917565679974));
#8738=CARTESIAN_POINT('Origin',(2.49048674522936,-0.48,2.28211064313085));
#8739=CARTESIAN_POINT('Origin',(2.49048674522936,0.48,2.28211064313085));
#8740=CARTESIAN_POINT('Origin',(2.49048674522936,0.48,2.28211064313085));
#8741=CARTESIAN_POINT('',(0.,0.,0.));
#8742=CARTESIAN_POINT('',(0.,0.,0.));
#8743=CARTESIAN_POINT('',(0.,0.,0.));
#8744=CARTESIAN_POINT('Origin',(11.4,0.,2.5));
#8745=CARTESIAN_POINT('',(11.4,-4.163799117101E-17,2.84));
#8746=CARTESIAN_POINT('Origin',(11.4,0.,2.5));
#8747=CARTESIAN_POINT('',(13.,4.163799117101E-17,2.84));
#8748=CARTESIAN_POINT('',(11.4,-4.163799117101E-17,2.84));
#8749=CARTESIAN_POINT('Origin',(13.,0.,2.5));
#8750=CARTESIAN_POINT('Origin',(11.4,0.,2.5));
#8751=CARTESIAN_POINT('Origin',(5.98369790806552,-1.,2.5));
#8752=CARTESIAN_POINT('',(5.67369790806552,-0.9,2.5));
#8753=CARTESIAN_POINT('Origin',(5.98369790806552,-0.9,2.5));
#8754=CARTESIAN_POINT('',(5.67369790806552,-0.5,2.5));
#8755=CARTESIAN_POINT('',(5.67369790806552,-1.,2.5));
#8756=CARTESIAN_POINT('Origin',(5.98369790806552,-0.5,2.5));
#8757=CARTESIAN_POINT('Origin',(5.98369790806552,-1.,2.5));
#8758=CARTESIAN_POINT('',(5.67369790806552,0.5,2.5));
#8759=CARTESIAN_POINT('Origin',(5.98369790806552,0.5,2.5));
#8760=CARTESIAN_POINT('',(5.67369790806552,0.9,2.5));
#8761=CARTESIAN_POINT('',(5.67369790806552,-1.,2.5));
#8762=CARTESIAN_POINT('Origin',(5.98369790806552,0.9,2.5));
#8763=CARTESIAN_POINT('Origin',(6.88369790806552,-0.9,1.7));
#8764=CARTESIAN_POINT('',(6.88369790806552,0.5,1.7));
#8765=CARTESIAN_POINT('',(6.88369790806552,0.5,3.3));
#8766=CARTESIAN_POINT('',(6.88369790806552,0.5,2.1));
#8767=CARTESIAN_POINT('',(6.88369790806552,-0.5,1.7));
#8768=CARTESIAN_POINT('',(6.88369790806552,-0.9,1.7));
#8769=CARTESIAN_POINT('',(6.88369790806552,-0.5,3.3));
#8770=CARTESIAN_POINT('',(6.88369790806552,-0.5,2.1));
#8771=CARTESIAN_POINT('',(6.88369790806552,-0.9,3.3));
#8772=CARTESIAN_POINT('Origin',(6.18369790806552,0.9,2.5));
#8773=CARTESIAN_POINT('',(7.18369790806552,0.9,1.7));
#8774=CARTESIAN_POINT('',(5.18369790806552,0.9,1.7));
#8775=CARTESIAN_POINT('',(5.18369790806552,0.9,1.7));
#8776=CARTESIAN_POINT('',(5.18369790806552,0.9,3.3));
#8777=CARTESIAN_POINT('',(5.18369790806552,0.9,3.3));
#8778=CARTESIAN_POINT('',(7.18369790806552,0.9,3.3));
#8779=CARTESIAN_POINT('',(7.18369790806552,0.9,3.3));
#8780=CARTESIAN_POINT('',(7.18369790806552,0.9,1.7));
#8781=CARTESIAN_POINT('Origin',(7.18369790806552,0.5,1.7));
#8782=CARTESIAN_POINT('',(5.18369790806552,0.5,1.7));
#8783=CARTESIAN_POINT('',(5.18369790806552,0.5,1.7));
#8784=CARTESIAN_POINT('',(5.18369790806552,0.5,1.7));
#8785=CARTESIAN_POINT('',(7.18369790806552,-0.9,1.7));
#8786=CARTESIAN_POINT('',(7.18369790806552,0.5,1.7));
#8787=CARTESIAN_POINT('',(5.18369790806552,-0.9,1.7));
#8788=CARTESIAN_POINT('',(5.18369790806552,-0.9,1.7));
#8789=CARTESIAN_POINT('',(5.18369790806552,-0.5,1.7));
#8790=CARTESIAN_POINT('',(5.18369790806552,-0.9,1.7));
#8791=CARTESIAN_POINT('',(5.18369790806552,-0.5,1.7));
#8792=CARTESIAN_POINT('Origin',(6.18369790806552,-0.9,2.5));
#8793=CARTESIAN_POINT('',(7.18369790806552,-0.9,3.3));
#8794=CARTESIAN_POINT('',(5.18369790806552,-0.9,3.3));
#8795=CARTESIAN_POINT('',(7.18369790806552,-0.9,3.3));
#8796=CARTESIAN_POINT('',(5.18369790806552,-0.9,3.3));
#8797=CARTESIAN_POINT('',(7.18369790806552,-0.9,1.7));
#8798=CARTESIAN_POINT('Origin',(5.18369790806552,0.5,1.7));
#8799=CARTESIAN_POINT('',(5.18369790806552,0.5,3.3));
#8800=CARTESIAN_POINT('',(5.18369790806552,0.5,3.3));
#8801=CARTESIAN_POINT('',(5.18369790806552,0.5,3.3));
#8802=CARTESIAN_POINT('Origin',(7.18369790806552,0.5,3.3));
#8803=CARTESIAN_POINT('',(7.18369790806552,0.5,3.3));
#8804=CARTESIAN_POINT('',(7.18369790806552,-6.12323399573677E-17,3.));
#8805=CARTESIAN_POINT('Origin',(7.18369790806552,0.,2.5));
#8806=CARTESIAN_POINT('Origin',(5.18369790806552,0.5,3.3));
#8807=CARTESIAN_POINT('',(7.18369790806552,0.5,3.3));
#8808=CARTESIAN_POINT('',(5.18369790806552,-0.5,3.3));
#8809=CARTESIAN_POINT('',(7.18369790806552,-0.5,3.3));
#8810=CARTESIAN_POINT('',(5.18369790806552,-0.9,3.3));
#8811=CARTESIAN_POINT('Origin',(6.18369790806552,0.5,2.5));
#8812=CARTESIAN_POINT('Origin',(5.18369790806552,-0.9,1.7));
#8813=CARTESIAN_POINT('',(5.18369790806552,-0.5,3.3));
#8814=CARTESIAN_POINT('Origin',(6.18369790806552,-0.5,2.5));
#8815=CARTESIAN_POINT('Origin',(6.98369791,0.,2.5));
#8816=CARTESIAN_POINT('',(13.,-6.12323399573677E-17,3.));
#8817=CARTESIAN_POINT('Origin',(13.,0.,2.5));
#8818=CARTESIAN_POINT('',(6.98369791,-6.12323399573677E-17,3.));
#8819=CARTESIAN_POINT('Origin',(13.,0.,2.5));
#8820=CARTESIAN_POINT('',(0.,0.,0.));
#8821=CARTESIAN_POINT('Origin',(0.,-1.935,0.));
#8822=CARTESIAN_POINT('',(-0.3933,-3.9267,4.81653586104654E-17));
#8823=CARTESIAN_POINT('Origin',(0.,-3.9267,0.));
#8824=CARTESIAN_POINT('',(-0.3933,0.,-4.81653586104654E-17));
#8825=CARTESIAN_POINT('',(-0.3933,-1.935,-4.81653586104654E-17));
#8826=CARTESIAN_POINT('Origin',(0.,0.,0.));
#8827=CARTESIAN_POINT('Origin',(0.,-3.96,0.));
#8828=CARTESIAN_POINT('',(-0.32,-4.,-3.91886975727153E-17));
#8829=CARTESIAN_POINT('Origin',(0.,-4.,0.));
#8830=CARTESIAN_POINT('',(-0.36,-3.96,-4.40872847693047E-17));
#8831=CARTESIAN_POINT('Origin',(0.,-4.,0.));
#8832=CARTESIAN_POINT('Origin',(0.,0.462722715486149,0.));
#8833=CARTESIAN_POINT('',(-0.6175,0.53,-7.5621939847349E-17));
#8834=CARTESIAN_POINT('Origin',(0.,0.53,0.));
#8835=CARTESIAN_POINT('',(-0.750555349946514,0.453180457891261,-9.19165206894919E-17));
#8836=CARTESIAN_POINT('',(-0.734027674973257,0.462722715486149,-8.98924642641573E-17));
#8837=CARTESIAN_POINT('',(-0.375277674973257,0.453180457891261,0.65));
#8838=CARTESIAN_POINT('Ctrl Pts',(-0.375277674973257,0.45318045789126,0.65));
#8839=CARTESIAN_POINT('Ctrl Pts',(-0.562916512459968,0.561513791224244,
0.324999999999856));
#8840=CARTESIAN_POINT('Ctrl Pts',(-0.750555349946514,0.45318045789126,-9.19165206894919E-17));
#8841=CARTESIAN_POINT('',(0.375277674973257,0.453180457891261,0.65));
#8842=CARTESIAN_POINT('Ctrl Pts',(0.375277674973257,0.453180457891261,0.65));
#8843=CARTESIAN_POINT('Ctrl Pts',(-1.66922031752392E-13,0.561513791224244,
0.65));
#8844=CARTESIAN_POINT('Ctrl Pts',(-0.375277674973257,0.45318045789126,0.65));
#8845=CARTESIAN_POINT('',(0.750555349946514,0.453180457891261,0.));
#8846=CARTESIAN_POINT('Ctrl Pts',(0.750555349946514,0.453180457891261,0.));
#8847=CARTESIAN_POINT('Ctrl Pts',(0.562916512459802,0.561513791224244,0.325000000000144));
#8848=CARTESIAN_POINT('Ctrl Pts',(0.375277674973257,0.45318045789126,0.65));
#8849=CARTESIAN_POINT('',(0.375277674973257,0.453180457891261,-0.65));
#8850=CARTESIAN_POINT('Ctrl Pts',(0.375277674973257,0.45318045789126,-0.65));
#8851=CARTESIAN_POINT('Ctrl Pts',(0.562916512459968,0.561513791224244,-0.324999999999855));
#8852=CARTESIAN_POINT('Ctrl Pts',(0.750555349946514,0.453180457891261,0.));
#8853=CARTESIAN_POINT('',(-0.375277674973257,0.45318045789126,-0.65));
#8854=CARTESIAN_POINT('Ctrl Pts',(-0.375277674973257,0.453180457891261,
-0.65));
#8855=CARTESIAN_POINT('Ctrl Pts',(1.66866520601161E-13,0.561513791224244,
-0.65));
#8856=CARTESIAN_POINT('Ctrl Pts',(0.375277674973257,0.45318045789126,-0.65));
#8857=CARTESIAN_POINT('Ctrl Pts',(-0.750555349946514,0.453180457891261,
-9.19165206894919E-17));
#8858=CARTESIAN_POINT('Ctrl Pts',(-0.562916512459802,0.561513791224244,
-0.325000000000144));
#8859=CARTESIAN_POINT('Ctrl Pts',(-0.375277674973257,0.45318045789126,-0.65));
#8860=CARTESIAN_POINT('Origin',(0.375277674973257,0.,-0.65));
#8861=CARTESIAN_POINT('',(0.375277674973257,0.,-0.65));
#8862=CARTESIAN_POINT('',(0.375277674973257,0.,-0.65));
#8863=CARTESIAN_POINT('',(-0.375277674973257,0.,-0.65));
#8864=CARTESIAN_POINT('',(0.375277674973257,0.,-0.65));
#8865=CARTESIAN_POINT('',(-0.375277674973257,0.,-0.65));
#8866=CARTESIAN_POINT('Origin',(0.750555349946514,0.,0.));
#8867=CARTESIAN_POINT('',(0.750555349946514,0.,0.));
#8868=CARTESIAN_POINT('',(0.750555349946514,0.,0.));
#8869=CARTESIAN_POINT('',(0.750555349946514,0.,0.));
#8870=CARTESIAN_POINT('Origin',(0.375277674973257,0.,0.65));
#8871=CARTESIAN_POINT('',(0.375277674973257,0.,0.65));
#8872=CARTESIAN_POINT('',(0.375277674973257,0.,0.65));
#8873=CARTESIAN_POINT('',(0.375277674973257,0.,0.65));
#8874=CARTESIAN_POINT('Origin',(-0.375277674973257,0.,0.65));
#8875=CARTESIAN_POINT('',(-0.375277674973257,0.,0.65));
#8876=CARTESIAN_POINT('',(-0.375277674973257,0.,0.65));
#8877=CARTESIAN_POINT('',(-0.375277674973257,0.,0.65));
#8878=CARTESIAN_POINT('Origin',(-0.750555349946514,0.,-9.19165206894919E-17));
#8879=CARTESIAN_POINT('',(-0.750555349946514,0.,-9.19165206894919E-17));
#8880=CARTESIAN_POINT('',(-0.750555349946514,0.,-9.19165206894919E-17));
#8881=CARTESIAN_POINT('',(-0.750555349946514,0.,-9.19165206894919E-17));
#8882=CARTESIAN_POINT('Origin',(-0.375277674973257,0.,-0.65));
#8883=CARTESIAN_POINT('',(-0.375277674973257,0.,-0.65));
#8884=CARTESIAN_POINT('Origin',(0.,0.53,-1.11022302462516E-16));
#8885=CARTESIAN_POINT('Origin',(0.,0.,-1.11022302462516E-16));
#8886=CARTESIAN_POINT('',(0.,0.,0.));
#8887=CARTESIAN_POINT('Origin',(0.,0.067277284513851,0.));
#8888=CARTESIAN_POINT('',(-0.375277674973257,0.0768195421087395,0.65));
#8889=CARTESIAN_POINT('',(0.375277674973257,0.0768195421087395,0.65));
#8890=CARTESIAN_POINT('Ctrl Pts',(-0.375277674973257,0.0768195421087395,
0.65));
#8891=CARTESIAN_POINT('Ctrl Pts',(1.66533453693773E-13,-0.0315137912242439,
0.65));
#8892=CARTESIAN_POINT('Ctrl Pts',(0.375277674973257,0.0768195421087394,
0.65));
#8893=CARTESIAN_POINT('',(-0.750555349946514,0.0768195421087394,-9.19165206894919E-17));
#8894=CARTESIAN_POINT('Ctrl Pts',(-0.750555349946514,0.0768195421087394,
-9.19165206894919E-17));
#8895=CARTESIAN_POINT('Ctrl Pts',(-0.562916512459802,-0.0315137912242434,
0.325000000000144));
#8896=CARTESIAN_POINT('Ctrl Pts',(-0.375277674973257,0.0768195421087395,
0.65));
#8897=CARTESIAN_POINT('',(-0.6175,-2.77555756156289E-17,-7.5621939847349E-17));
#8898=CARTESIAN_POINT('',(-0.734027674973257,0.067277284513851,-8.98924642641573E-17));
#8899=CARTESIAN_POINT('Origin',(0.,0.,0.));
#8900=CARTESIAN_POINT('',(-0.375277674973257,0.0768195421087395,-0.65));
#8901=CARTESIAN_POINT('Ctrl Pts',(-0.375277674973257,0.0768195421087395,
-0.65));
#8902=CARTESIAN_POINT('Ctrl Pts',(-0.562916512459968,-0.0315137912242437,
-0.324999999999856));
#8903=CARTESIAN_POINT('Ctrl Pts',(-0.750555349946514,0.0768195421087395,
-9.19165206894919E-17));
#8904=CARTESIAN_POINT('',(0.375277674973257,0.0768195421087395,-0.65));
#8905=CARTESIAN_POINT('Ctrl Pts',(0.375277674973257,0.0768195421087395,
-0.65));
#8906=CARTESIAN_POINT('Ctrl Pts',(-1.66144875635155E-13,-0.0315137912242437,
-0.65));
#8907=CARTESIAN_POINT('Ctrl Pts',(-0.375277674973257,0.0768195421087395,
-0.65));
#8908=CARTESIAN_POINT('',(0.750555349946514,0.0768195421087394,0.));
#8909=CARTESIAN_POINT('Ctrl Pts',(0.750555349946514,0.0768195421087394,
0.));
#8910=CARTESIAN_POINT('Ctrl Pts',(0.562916512459802,-0.0315137912242436,
-0.325000000000144));
#8911=CARTESIAN_POINT('Ctrl Pts',(0.375277674973257,0.0768195421087395,
-0.65));
#8912=CARTESIAN_POINT('Ctrl Pts',(0.375277674973257,0.0768195421087394,
0.65));
#8913=CARTESIAN_POINT('Ctrl Pts',(0.562916512459968,-0.0315137912242439,
0.324999999999856));
#8914=CARTESIAN_POINT('Ctrl Pts',(0.750555349946514,0.0768195421087394,
0.));
#8915=CARTESIAN_POINT('Origin',(0.,0.612722715486149,0.));
#8916=CARTESIAN_POINT('',(-0.6175,0.68,-7.5621939847349E-17));
#8917=CARTESIAN_POINT('Origin',(0.,0.68,0.));
#8918=CARTESIAN_POINT('',(-0.750555349946514,0.603180457891261,-9.19165206894919E-17));
#8919=CARTESIAN_POINT('',(-0.734027674973257,0.612722715486149,-8.98924642641573E-17));
#8920=CARTESIAN_POINT('',(-0.375277674973257,0.603180457891261,0.65));
#8921=CARTESIAN_POINT('Ctrl Pts',(-0.375277674973257,0.603180457891261,
0.65));
#8922=CARTESIAN_POINT('Ctrl Pts',(-0.562916512459968,0.711513791224243,
0.324999999999856));
#8923=CARTESIAN_POINT('Ctrl Pts',(-0.750555349946514,0.603180457891261,
-9.19165206894919E-17));
#8924=CARTESIAN_POINT('',(0.375277674973257,0.603180457891261,0.65));
#8925=CARTESIAN_POINT('Ctrl Pts',(0.375277674973257,0.603180457891261,0.65));
#8926=CARTESIAN_POINT('Ctrl Pts',(-1.66755498298699E-13,0.711513791224244,
0.65));
#8927=CARTESIAN_POINT('Ctrl Pts',(-0.375277674973257,0.603180457891261,
0.65));
#8928=CARTESIAN_POINT('',(0.750555349946514,0.603180457891261,0.));
#8929=CARTESIAN_POINT('Ctrl Pts',(0.750555349946514,0.603180457891261,0.));
#8930=CARTESIAN_POINT('Ctrl Pts',(0.562916512459802,0.711513791224244,0.325000000000144));
#8931=CARTESIAN_POINT('Ctrl Pts',(0.375277674973257,0.603180457891261,0.65));
#8932=CARTESIAN_POINT('',(0.375277674973257,0.603180457891261,-0.65));
#8933=CARTESIAN_POINT('Ctrl Pts',(0.375277674973257,0.603180457891261,-0.65));
#8934=CARTESIAN_POINT('Ctrl Pts',(0.562916512459969,0.711513791224244,-0.324999999999856));
#8935=CARTESIAN_POINT('Ctrl Pts',(0.750555349946514,0.603180457891261,0.));
#8936=CARTESIAN_POINT('',(-0.375277674973257,0.603180457891261,-0.65));
#8937=CARTESIAN_POINT('Ctrl Pts',(-0.375277674973257,0.603180457891261,
-0.65));
#8938=CARTESIAN_POINT('Ctrl Pts',(1.66422431391311E-13,0.711513791224244,
-0.65));
#8939=CARTESIAN_POINT('Ctrl Pts',(0.375277674973257,0.603180457891261,-0.65));
#8940=CARTESIAN_POINT('Ctrl Pts',(-0.750555349946514,0.603180457891261,
-9.19165206894919E-17));
#8941=CARTESIAN_POINT('Ctrl Pts',(-0.562916512459802,0.711513791224244,
-0.325000000000144));
#8942=CARTESIAN_POINT('Ctrl Pts',(-0.375277674973257,0.603180457891261,
-0.65));
#8943=CARTESIAN_POINT('Origin',(0.375277674973257,0.,-0.65));
#8944=CARTESIAN_POINT('',(-0.375277674973257,0.,-0.65));
#8945=CARTESIAN_POINT('',(0.375277674973257,0.,-0.65));
#8946=CARTESIAN_POINT('Origin',(-0.375277674973257,0.,-0.65));
#8947=CARTESIAN_POINT('',(-0.750555349946514,0.,-9.19165206894919E-17));
#8948=CARTESIAN_POINT('Origin',(-0.750555349946514,0.,-9.19165206894919E-17));
#8949=CARTESIAN_POINT('',(-0.375277674973257,0.,0.65));
#8950=CARTESIAN_POINT('Origin',(0.,0.,0.));
#8951=CARTESIAN_POINT('',(-0.338975,0.68,4.15124648740974E-17));
#8952=CARTESIAN_POINT('Origin',(0.,0.68,0.));
#8953=CARTESIAN_POINT('',(-0.338975,0.,4.15124648740974E-17));
#8954=CARTESIAN_POINT('',(-0.338975,0.,4.15124648740974E-17));
#8955=CARTESIAN_POINT('Origin',(0.,0.,0.));
#8956=CARTESIAN_POINT('Origin',(-0.375277674973257,0.,0.65));
#8957=CARTESIAN_POINT('',(0.375277674973257,0.,0.65));
#8958=CARTESIAN_POINT('Origin',(0.750555349946514,0.,0.));
#8959=CARTESIAN_POINT('',(0.750555349946514,0.,0.));
#8960=CARTESIAN_POINT('Origin',(0.375277674973257,0.,0.65));
#8961=CARTESIAN_POINT('Origin',(0.,0.68,-1.11022302462516E-16));
#8962=CARTESIAN_POINT('Origin',(0.,0.,-1.11022302462516E-16));
#8963=CARTESIAN_POINT('',(0.,0.,0.));
#8964=CARTESIAN_POINT('Origin',(0.,0.,3.));
#8965=CARTESIAN_POINT('',(-1.,-1.22464679914735E-16,3.4));
#8966=CARTESIAN_POINT('Origin',(0.,0.,3.4));
#8967=CARTESIAN_POINT('',(-1.,-1.22464679914735E-16,3.));
#8968=CARTESIAN_POINT('',(-1.,-1.22464679914735E-16,3.));
#8969=CARTESIAN_POINT('Origin',(0.,0.,3.));
#8970=CARTESIAN_POINT('Origin',(0.,0.,3.4));
#8971=CARTESIAN_POINT('Origin',(0.,0.,3.));
#8972=CARTESIAN_POINT('',(0.,0.,0.));
#8973=CARTESIAN_POINT('Origin',(0.,-2.7,0.));
#8974=CARTESIAN_POINT('',(-0.289136645896019,-2.7,0.08));
#8975=CARTESIAN_POINT('',(-0.3,-2.78,-2.27065106771523E-17));
#8976=CARTESIAN_POINT('Ctrl Pts',(-0.289136645896019,-2.7,0.08));
#8977=CARTESIAN_POINT('Ctrl Pts',(-0.289136645896019,-2.71009877520201,
0.08));
#8978=CARTESIAN_POINT('Ctrl Pts',(-0.289720927595908,-2.72083518625944,
0.0779717130936404));
#8979=CARTESIAN_POINT('Ctrl Pts',(-0.291799203044223,-2.74052980652726,
0.0697927537456149));
#8980=CARTESIAN_POINT('Ctrl Pts',(-0.293259762986909,-2.74949254880105,
0.0636445361887959));
#8981=CARTESIAN_POINT('Ctrl Pts',(-0.295976783522942,-2.76364324458222,
0.0494938404076284));
#8982=CARTESIAN_POINT('Ctrl Pts',(-0.297414335384467,-2.76979246713824,
0.0405305642602551));
#8983=CARTESIAN_POINT('Ctrl Pts',(-0.299439403644655,-2.77797216257078,
0.0208340363410407));
#8984=CARTESIAN_POINT('Ctrl Pts',(-0.3,-2.78,0.0100969318362556));
#8985=CARTESIAN_POINT('Ctrl Pts',(-0.3,-2.78,5.20417042793042E-18));
#8986=CARTESIAN_POINT('',(0.289136645896019,-2.7,0.08));
#8987=CARTESIAN_POINT('',(0.,-2.7,0.08));
#8988=CARTESIAN_POINT('Ctrl Pts',(0.289136645896019,-2.7,0.08));
#8989=CARTESIAN_POINT('Ctrl Pts',(0.289136645896019,-2.68990122479799,0.08));
#8990=CARTESIAN_POINT('Ctrl Pts',(0.289720927595908,-2.67916481374056,0.0779717130936404));
#8991=CARTESIAN_POINT('Ctrl Pts',(0.291799203044223,-2.65947019347274,0.0697927537456147));
#8992=CARTESIAN_POINT('Ctrl Pts',(0.293259762986909,-2.65050745119895,0.0636445361887959));
#8993=CARTESIAN_POINT('Ctrl Pts',(0.295976783522942,-2.63635675541778,0.0494938404076283));
#8994=CARTESIAN_POINT('Ctrl Pts',(0.297414335384467,-2.63020753286176,0.0405305642602551));
#8995=CARTESIAN_POINT('Ctrl Pts',(0.299439403644655,-2.62202783742922,0.0208340363410406));
#8996=CARTESIAN_POINT('Ctrl Pts',(0.3,-2.62,0.0100969318362555));
#8997=CARTESIAN_POINT('Ctrl Pts',(0.3,-2.62,-0.0100969318362556));
#8998=CARTESIAN_POINT('Ctrl Pts',(0.299439403644655,-2.62202783742922,-0.0208340363410406));
#8999=CARTESIAN_POINT('Ctrl Pts',(0.297414335384467,-2.63020753286176,-0.0405305642602551));
#9000=CARTESIAN_POINT('Ctrl Pts',(0.295976783522942,-2.63635675541778,-0.0494938404076283));
#9001=CARTESIAN_POINT('Ctrl Pts',(0.293259762986909,-2.65050745119895,-0.0636445361887959));
#9002=CARTESIAN_POINT('Ctrl Pts',(0.291799203044223,-2.65947019347274,-0.0697927537456147));
#9003=CARTESIAN_POINT('Ctrl Pts',(0.289720927595908,-2.67916481374056,-0.0779717130936403));
#9004=CARTESIAN_POINT('Ctrl Pts',(0.289136645896019,-2.68990122479799,-0.08));
#9005=CARTESIAN_POINT('Ctrl Pts',(0.289136645896019,-2.71009877520201,-0.08));
#9006=CARTESIAN_POINT('Ctrl Pts',(0.289720927595908,-2.72083518625944,-0.0779717130936404));
#9007=CARTESIAN_POINT('Ctrl Pts',(0.291799203044223,-2.74052980652726,-0.0697927537456147));
#9008=CARTESIAN_POINT('Ctrl Pts',(0.293259762986909,-2.74949254880105,-0.0636445361887959));
#9009=CARTESIAN_POINT('Ctrl Pts',(0.295976783522942,-2.76364324458222,-0.0494938404076283));
#9010=CARTESIAN_POINT('Ctrl Pts',(0.297414335384467,-2.76979246713824,-0.0405305642602551));
#9011=CARTESIAN_POINT('Ctrl Pts',(0.299439403644655,-2.77797216257078,-0.0208340363410406));
#9012=CARTESIAN_POINT('Ctrl Pts',(0.3,-2.78,-0.0100969318362555));
#9013=CARTESIAN_POINT('Ctrl Pts',(0.3,-2.78,0.0100969318362556));
#9014=CARTESIAN_POINT('Ctrl Pts',(0.299439403644655,-2.77797216257078,0.0208340363410407));
#9015=CARTESIAN_POINT('Ctrl Pts',(0.297414335384467,-2.76979246713824,0.0405305642602551));
#9016=CARTESIAN_POINT('Ctrl Pts',(0.295976783522942,-2.76364324458222,0.0494938404076284));
#9017=CARTESIAN_POINT('Ctrl Pts',(0.293259762986909,-2.74949254880105,0.0636445361887959));
#9018=CARTESIAN_POINT('Ctrl Pts',(0.291799203044223,-2.74052980652726,0.0697927537456149));
#9019=CARTESIAN_POINT('Ctrl Pts',(0.289720927595908,-2.72083518625944,0.0779717130936404));
#9020=CARTESIAN_POINT('Ctrl Pts',(0.289136645896019,-2.71009877520201,0.08));
#9021=CARTESIAN_POINT('Ctrl Pts',(0.289136645896019,-2.7,0.08));
#9022=CARTESIAN_POINT('',(-0.3,-2.62,-3.65842984849668E-17));
#9023=CARTESIAN_POINT('Ctrl Pts',(-0.3,-2.62,-3.81639164714898E-17));
#9024=CARTESIAN_POINT('Ctrl Pts',(-0.3,-2.62,0.0100969318362555));
#9025=CARTESIAN_POINT('Ctrl Pts',(-0.299439403644655,-2.62202783742922,
0.0208340363410406));
#9026=CARTESIAN_POINT('Ctrl Pts',(-0.297414335384467,-2.63020753286176,
0.040530564260255));
#9027=CARTESIAN_POINT('Ctrl Pts',(-0.295976783522942,-2.63635675541778,
0.0494938404076283));
#9028=CARTESIAN_POINT('Ctrl Pts',(-0.293259762986909,-2.65050745119895,
0.0636445361887959));
#9029=CARTESIAN_POINT('Ctrl Pts',(-0.291799203044223,-2.65947019347274,
0.0697927537456147));
#9030=CARTESIAN_POINT('Ctrl Pts',(-0.289720927595908,-2.67916481374056,
0.0779717130936404));
#9031=CARTESIAN_POINT('Ctrl Pts',(-0.289136645896019,-2.68990122479799,
0.08));
#9032=CARTESIAN_POINT('Ctrl Pts',(-0.289136645896019,-2.7,0.08));
#9033=CARTESIAN_POINT('Ctrl Pts',(-0.3,-2.78,-6.93889390390723E-18));
#9034=CARTESIAN_POINT('Ctrl Pts',(-0.3,-2.78,-0.0100969318362556));
#9035=CARTESIAN_POINT('Ctrl Pts',(-0.299439403644655,-2.77797216257078,
-0.0208340363410406));
#9036=CARTESIAN_POINT('Ctrl Pts',(-0.297414335384467,-2.76979246713824,
-0.0405305642602551));
#9037=CARTESIAN_POINT('Ctrl Pts',(-0.295976783522942,-2.76364324458222,
-0.0494938404076283));
#9038=CARTESIAN_POINT('Ctrl Pts',(-0.293259762986909,-2.74949254880105,
-0.0636445361887959));
#9039=CARTESIAN_POINT('Ctrl Pts',(-0.291799203044223,-2.74052980652726,
-0.0697927537456147));
#9040=CARTESIAN_POINT('Ctrl Pts',(-0.289720927595908,-2.72083518625944,
-0.0779717130936403));
#9041=CARTESIAN_POINT('Ctrl Pts',(-0.289136645896019,-2.71009877520201,
-0.08));
#9042=CARTESIAN_POINT('Ctrl Pts',(-0.289136645896019,-2.68990122479799,
-0.08));
#9043=CARTESIAN_POINT('Ctrl Pts',(-0.289720927595908,-2.67916481374056,
-0.0779717130936403));
#9044=CARTESIAN_POINT('Ctrl Pts',(-0.291799203044223,-2.65947019347274,
-0.0697927537456147));
#9045=CARTESIAN_POINT('Ctrl Pts',(-0.293259762986909,-2.65050745119895,
-0.0636445361887959));
#9046=CARTESIAN_POINT('Ctrl Pts',(-0.295976783522942,-2.63635675541778,
-0.0494938404076283));
#9047=CARTESIAN_POINT('Ctrl Pts',(-0.297414335384467,-2.63020753286176,
-0.0405305642602551));
#9048=CARTESIAN_POINT('Ctrl Pts',(-0.299439403644655,-2.62202783742922,
-0.0208340363410406));
#9049=CARTESIAN_POINT('Ctrl Pts',(-0.3,-2.62,-0.0100969318362556));
#9050=CARTESIAN_POINT('Ctrl Pts',(-0.3,-2.62,-1.56125112837913E-17));
#9051=CARTESIAN_POINT('Origin',(0.45,0.2,0.));
#9052=CARTESIAN_POINT('',(-0.45,0.2,-5.51091059616309E-17));
#9053=CARTESIAN_POINT('Origin',(0.,0.2,0.));
#9054=CARTESIAN_POINT('Origin',(0.,0.175,0.));
#9055=CARTESIAN_POINT('',(-0.5,0.15,-6.12323399573676E-17));
#9056=CARTESIAN_POINT('Origin',(0.,0.15,0.));
#9057=CARTESIAN_POINT('',(-0.475,0.175,-5.81707229594993E-17));
#9058=CARTESIAN_POINT('Origin',(0.,0.0750000000000002,0.));
#9059=CARTESIAN_POINT('',(-0.5,0.,-6.12323399573677E-17));
#9060=CARTESIAN_POINT('Origin',(0.,0.,0.));
#9061=CARTESIAN_POINT('',(-0.5,0.0750000000000002,-6.12323399573677E-17));
#9062=CARTESIAN_POINT('Origin',(0.3,0.,0.));
#9063=CARTESIAN_POINT('',(-0.3,0.,-3.67394039744206E-17));
#9064=CARTESIAN_POINT('Origin',(0.,0.,0.));
#9065=CARTESIAN_POINT('Origin',(0.,-1.455,0.));
#9066=CARTESIAN_POINT('',(-0.3,-2.91,-3.67394039744206E-17));
#9067=CARTESIAN_POINT('Origin',(0.,-2.91,0.));
#9068=CARTESIAN_POINT('',(-0.3,-1.455,-3.67394039744206E-17));
#9069=CARTESIAN_POINT('',(-0.3,-1.455,-3.67394039744206E-17));
#9070=CARTESIAN_POINT('Origin',(0.,-2.955,0.));
#9071=CARTESIAN_POINT('',(-0.21,-3.,-2.57175827820944E-17));
#9072=CARTESIAN_POINT('Origin',(0.,-3.,0.));
#9073=CARTESIAN_POINT('',(-0.255,-2.955,-3.12284933782575E-17));
#9074=CARTESIAN_POINT('Origin',(0.,-3.,0.));
#9075=CARTESIAN_POINT('',(0.,0.,0.));
#9076=CARTESIAN_POINT('Origin',(0.,0.,0.));
#9077=CARTESIAN_POINT('',(-0.32,0.16,3.91886975727153E-17));
#9078=CARTESIAN_POINT('Origin',(0.,0.16,0.));
#9079=CARTESIAN_POINT('',(-0.32,0.,3.91886975727153E-17));
#9080=CARTESIAN_POINT('',(-0.32,0.,3.91886975727153E-17));
#9081=CARTESIAN_POINT('Origin',(0.,0.,0.));
#9082=CARTESIAN_POINT('Origin',(0.,0.,0.));
#9083=CARTESIAN_POINT('',(-0.6,0.16,7.34788079488412E-17));
#9084=CARTESIAN_POINT('Origin',(0.,0.16,0.));
#9085=CARTESIAN_POINT('',(-0.6,0.,7.34788079488412E-17));
#9086=CARTESIAN_POINT('',(-0.6,0.,7.34788079488412E-17));
#9087=CARTESIAN_POINT('Origin',(0.,0.,0.));
#9088=CARTESIAN_POINT('Origin',(0.,0.16,0.));
#9089=CARTESIAN_POINT('Origin',(0.,0.,0.));
#9090=CARTESIAN_POINT('',(0.,0.,0.));
#9091=CARTESIAN_POINT('Origin',(0.,-1.54,2.5));
#9092=CARTESIAN_POINT('',(-0.31,-1.06,2.5));
#9093=CARTESIAN_POINT('Origin',(0.,-1.06,2.5));
#9094=CARTESIAN_POINT('',(-0.31,-1.54,2.5));
#9095=CARTESIAN_POINT('',(-0.31,-1.54,2.5));
#9096=CARTESIAN_POINT('Origin',(0.,-1.54,2.5));
#9097=CARTESIAN_POINT('Origin',(0.,-1.54,2.5));
#9098=CARTESIAN_POINT('',(-0.5,-1.06,2.5));
#9099=CARTESIAN_POINT('Origin',(0.,-1.06,2.5));
#9100=CARTESIAN_POINT('',(-0.5,-1.54,2.5));
#9101=CARTESIAN_POINT('',(-0.5,-1.54,2.5));
#9102=CARTESIAN_POINT('Origin',(0.,-1.54,2.5));
#9103=CARTESIAN_POINT('Origin',(0.,-1.06,2.5));
#9104=CARTESIAN_POINT('Origin',(0.,-1.54,2.5));
#9105=CARTESIAN_POINT('',(0.,0.,0.));
#9106=CARTESIAN_POINT('Origin',(0.,0.12,0.));
#9107=CARTESIAN_POINT('',(-9.79717439317883E-18,0.12,-0.04));
#9108=CARTESIAN_POINT('Origin',(0.,0.12,-0.12));
#9109=CARTESIAN_POINT('Origin',(9.79717439317883E-18,0.12,0.));
#9110=CARTESIAN_POINT('',(0.08,-4.89858719658941E-18,7.34788079488412E-18));
#9111=CARTESIAN_POINT('',(-0.08,-4.89858719658941E-18,7.34788079488412E-18));
#9112=CARTESIAN_POINT('Ctrl Pts',(0.08,-4.89858719658941E-18,7.34788079488412E-18));
#9113=CARTESIAN_POINT('Ctrl Pts',(0.08,-0.00012864962353541,0.000128649623535413));
#9114=CARTESIAN_POINT('Ctrl Pts',(0.0799996896739287,-0.00025719571182076,
0.000257402596003253));
#9115=CARTESIAN_POINT('Ctrl Pts',(0.0799669711262291,-0.00701193164572964,
0.00703384588894362));
#9116=CARTESIAN_POINT('Ctrl Pts',(0.0791054994909294,-0.0133457972655825,
0.0139383126556792));
#9117=CARTESIAN_POINT('Ctrl Pts',(0.0749700088488058,-0.0265076530862524,
0.0292212026164895));
#9118=CARTESIAN_POINT('Ctrl Pts',(0.0712702072865517,-0.0331317062461458,
0.0375603420117568));
#9119=CARTESIAN_POINT('Ctrl Pts',(0.0612858949407667,-0.0440683985740427,
0.0520545604187517));
#9120=CARTESIAN_POINT('Ctrl Pts',(0.0555090276731744,-0.0485199197794574,
0.0582717815295611));
#9121=CARTESIAN_POINT('Ctrl Pts',(0.0412398082144208,-0.0561090538733877,
0.0691638397919718));
#9122=CARTESIAN_POINT('Ctrl Pts',(0.0327878980890048,-0.059089642483296,
0.0736229049587921));
#9123=CARTESIAN_POINT('Ctrl Pts',(0.0159233027310102,-0.0625179833270725,
0.0787936360751706));
#9124=CARTESIAN_POINT('Ctrl Pts',(0.00801661414593076,-0.0633030277982336,
0.08));
#9125=CARTESIAN_POINT('Ctrl Pts',(-0.00801661414593074,-0.0633030277982336,
0.08));
#9126=CARTESIAN_POINT('Ctrl Pts',(-0.0159233027310102,-0.0625179833270726,
0.0787936360751706));
#9127=CARTESIAN_POINT('Ctrl Pts',(-0.0327878980890049,-0.059089642483296,
0.0736229049587921));
#9128=CARTESIAN_POINT('Ctrl Pts',(-0.0412398082144209,-0.0561090538733877,
0.0691638397919717));
#9129=CARTESIAN_POINT('Ctrl Pts',(-0.0555090276731744,-0.0485199197794574,
0.0582717815295611));
#9130=CARTESIAN_POINT('Ctrl Pts',(-0.0612858949407667,-0.0440683985740427,
0.0520545604187517));
#9131=CARTESIAN_POINT('Ctrl Pts',(-0.0712702072865517,-0.0331317062461458,
0.0375603420117568));
#9132=CARTESIAN_POINT('Ctrl Pts',(-0.0749700088488058,-0.0265076530862524,
0.0292212026164895));
#9133=CARTESIAN_POINT('Ctrl Pts',(-0.0791054994909264,-0.0133457972655921,
0.0139383126556903));
#9134=CARTESIAN_POINT('Ctrl Pts',(-0.0799669711262287,-0.00701193164579759,
0.0070338458890125));
#9135=CARTESIAN_POINT('Ctrl Pts',(-0.0799996896739287,-0.000257195711817665,
0.000257402596000083));
#9136=CARTESIAN_POINT('Ctrl Pts',(-0.08,-0.000128649623538514,0.000128649623538516));
#9137=CARTESIAN_POINT('Ctrl Pts',(-0.08,-4.89858719658941E-18,7.34788079488412E-18));
#9138=CARTESIAN_POINT('Ctrl Pts',(-0.08,-4.89858719658941E-18,7.34788079488412E-18));
#9139=CARTESIAN_POINT('Ctrl Pts',(-0.08,-0.000128649623536042,-0.00012864962353603));
#9140=CARTESIAN_POINT('Ctrl Pts',(-0.0799996896739287,-0.000257195711820127,
-0.000257402596002604));
#9141=CARTESIAN_POINT('Ctrl Pts',(-0.0799669711262289,-0.0070119316457589,
-0.00703384588897312));
#9142=CARTESIAN_POINT('Ctrl Pts',(-0.0791054994909281,-0.0133457972655867,
-0.0139383126556841));
#9143=CARTESIAN_POINT('Ctrl Pts',(-0.0749700088488058,-0.0265076530862525,
-0.0292212026164896));
#9144=CARTESIAN_POINT('Ctrl Pts',(-0.0712702072865516,-0.0331317062461459,
-0.0375603420117568));
#9145=CARTESIAN_POINT('Ctrl Pts',(-0.0612858949407667,-0.0440683985740427,
-0.0520545604187517));
#9146=CARTESIAN_POINT('Ctrl Pts',(-0.0555090276731744,-0.0485199197794574,
-0.0582717815295611));
#9147=CARTESIAN_POINT('Ctrl Pts',(-0.0412398082144209,-0.0561090538733877,
-0.0691638397919717));
#9148=CARTESIAN_POINT('Ctrl Pts',(-0.0327878980890049,-0.059089642483296,
-0.0736229049587921));
#9149=CARTESIAN_POINT('Ctrl Pts',(-0.0159233027310101,-0.0625179833270725,
-0.0787936360751706));
#9150=CARTESIAN_POINT('Ctrl Pts',(-0.00801661414593069,-0.0633030277982336,
-0.08));
#9151=CARTESIAN_POINT('Ctrl Pts',(0.0080166141459307,-0.0633030277982336,
-0.08));
#9152=CARTESIAN_POINT('Ctrl Pts',(0.0159233027310101,-0.0625179833270725,
-0.0787936360751706));
#9153=CARTESIAN_POINT('Ctrl Pts',(0.0327878980890049,-0.0590896424832959,
-0.0736229049587921));
#9154=CARTESIAN_POINT('Ctrl Pts',(0.0412398082144209,-0.0561090538733877,
-0.0691638397919717));
#9155=CARTESIAN_POINT('Ctrl Pts',(0.0555090276731744,-0.0485199197794574,
-0.0582717815295611));
#9156=CARTESIAN_POINT('Ctrl Pts',(0.0612858949407666,-0.0440683985740428,
-0.0520545604187518));
#9157=CARTESIAN_POINT('Ctrl Pts',(0.0712702072865517,-0.0331317062461458,
-0.0375603420117568));
#9158=CARTESIAN_POINT('Ctrl Pts',(0.0749700088488058,-0.0265076530862524,
-0.0292212026164895));
#9159=CARTESIAN_POINT('Ctrl Pts',(0.079105499490928,-0.013345797265587,
-0.0139383126556845));
#9160=CARTESIAN_POINT('Ctrl Pts',(0.0799669711262289,-0.00701193164576148,
-0.00703384588897579));
#9161=CARTESIAN_POINT('Ctrl Pts',(0.0799996896739287,-0.000257195711819584,
-0.000257402596002039));
#9162=CARTESIAN_POINT('Ctrl Pts',(0.08,-0.000128649623536605,-0.000128649623536593));
#9163=CARTESIAN_POINT('Ctrl Pts',(0.08,-4.89858719658941E-18,7.34788079488412E-18));
#9164=CARTESIAN_POINT('Origin',(0.04,-1.36,0.));
#9165=CARTESIAN_POINT('',(0.,-1.36,-0.08));
#9166=CARTESIAN_POINT('',(0.,-1.36,0.08));
#9167=CARTESIAN_POINT('Origin',(0.,-1.36,0.));
#9168=CARTESIAN_POINT('',(0.,-1.36,-0.04));
#9169=CARTESIAN_POINT('Origin',(0.,0.,-0.08));
#9170=CARTESIAN_POINT('',(0.,-1.6,0.08));
#9171=CARTESIAN_POINT('',(0.,0.,0.08));
#9172=CARTESIAN_POINT('',(0.,-1.6,-0.08));
#9173=CARTESIAN_POINT('',(0.,-1.6,-0.09));
#9174=CARTESIAN_POINT('',(0.,0.,-0.08));
#9175=CARTESIAN_POINT('Origin',(0.,0.,0.));
#9176=CARTESIAN_POINT('',(-0.08,-1.6,-9.79717439317883E-18));
#9177=CARTESIAN_POINT('Origin',(0.,-1.6,0.));
#9178=CARTESIAN_POINT('',(-0.08,0.,-9.79717439317883E-18));
#9179=CARTESIAN_POINT('Origin',(0.,-1.6,0.));
#9180=CARTESIAN_POINT('Origin',(-0.04,-1.6,0.));
#9181=CARTESIAN_POINT('',(0.,0.,0.));
#9182=CARTESIAN_POINT('',(0.,0.,0.));
#9183=CARTESIAN_POINT('',(0.,1.06,2.5));
#9184=CARTESIAN_POINT('',(0.,-1.06,2.5));
#9185=CARTESIAN_POINT('',(0.,0.9,2.5));
#9186=CARTESIAN_POINT('',(-0.4,-1.64,2.5));
#9187=CARTESIAN_POINT('',(0.,0.,0.));
#9188=CARTESIAN_POINT('',(-1.2,0.,0.6));
#9189=CARTESIAN_POINT('',(-1.2,0.,0.7));
#9190=CARTESIAN_POINT('',(10.5,0.,0.6));
#9191=CARTESIAN_POINT('',(10.5,0.,0.7));
#9192=CARTESIAN_POINT('',(0.,0.,0.));
#9193=CARTESIAN_POINT('',(0.,0.,0.));
#9194=CARTESIAN_POINT('',(0.,0.,0.));
#9195=CARTESIAN_POINT('',(18.,0.,-0.8));
#9196=CARTESIAN_POINT('',(20.3,0.,-0.8));
#9197=CARTESIAN_POINT('',(18.,0.,4.));
#9198=CARTESIAN_POINT('',(20.3,0.,4.));
#9199=CARTESIAN_POINT('',(0.,5.,0.));
#9200=CARTESIAN_POINT('',(0.,2.5,7.5));
#9201=CARTESIAN_POINT('',(17.3,-2.5,7.));
#9202=CARTESIAN_POINT('',(17.3,2.5,7.));
#9203=CARTESIAN_POINT('',(17.8,5.,4.5));
#9204=CARTESIAN_POINT('',(17.8,5.,7.));
#9205=CARTESIAN_POINT('',(0.,0.,0.));
#9206=CARTESIAN_POINT('',(0.435778713738291,6.2,-2.54902650954127));
#9207=CARTESIAN_POINT('',(0.435778713738291,0.3,7.48097349045873));
#9208=CARTESIAN_POINT('',(2.49048674522936,1.06,2.28211064313085));
#9209=CARTESIAN_POINT('',(2.49048674522936,-1.06,2.28211064313085));
#9210=CARTESIAN_POINT('',(2.49048674522936,0.9,2.28211064313085));
#9211=CARTESIAN_POINT('',(2.49048674522936,0.,-0.217889356869145));
#9212=CARTESIAN_POINT('',(2.09048674522936,-1.64,2.28211064313085));
#9213=CARTESIAN_POINT('',(0.,0.,0.));
#9214=CARTESIAN_POINT('',(15.5,0.,2.5));
#9215=CARTESIAN_POINT('',(13.,0.,2.5));
#9216=CARTESIAN_POINT('',(13.03,0.,2.5));
#9217=CARTESIAN_POINT('',(5.98369790806552,1.06,2.5));
#9218=CARTESIAN_POINT('',(5.98369790806552,-1.06,2.5));
#9219=CARTESIAN_POINT('',(5.98369790806552,0.9,2.5));
#9220=CARTESIAN_POINT('',(5.98369790806552,0.,0.));
#9221=CARTESIAN_POINT('',(5.58369790806552,-1.64,2.5));
#9222=CARTESIAN_POINT('',(0.,0.,0.));
#9223=CARTESIAN_POINT('',(0.,0.,0.));
#9224=CARTESIAN_POINT('',(0.,0.,0.));
#9225=CARTESIAN_POINT('',(0.,0.,0.));
#9226=UNCERTAINTY_MEASURE_WITH_UNIT(LENGTH_MEASURE(0.001),#9286,
'DISTANCE_ACCURACY_VALUE',
'Maximum model space distance between geometric entities at asserted c
onnectivities');
#9227=UNCERTAINTY_MEASURE_WITH_UNIT(LENGTH_MEASURE(0.001),#9286,
'DISTANCE_ACCURACY_VALUE',
'Maximum model space distance between geometric entities at asserted c
onnectivities');
#9228=UNCERTAINTY_MEASURE_WITH_UNIT(LENGTH_MEASURE(0.001),#9286,
'DISTANCE_ACCURACY_VALUE',
'Maximum model space distance between geometric entities at asserted c
onnectivities');
#9229=UNCERTAINTY_MEASURE_WITH_UNIT(LENGTH_MEASURE(0.001),#9286,
'DISTANCE_ACCURACY_VALUE',
'Maximum model space distance between geometric entities at asserted c
onnectivities');
#9230=UNCERTAINTY_MEASURE_WITH_UNIT(LENGTH_MEASURE(0.001),#9286,
'DISTANCE_ACCURACY_VALUE',
'Maximum model space distance between geometric entities at asserted c
onnectivities');
#9231=UNCERTAINTY_MEASURE_WITH_UNIT(LENGTH_MEASURE(0.001),#9286,
'DISTANCE_ACCURACY_VALUE',
'Maximum model space distance between geometric entities at asserted c
onnectivities');
#9232=UNCERTAINTY_MEASURE_WITH_UNIT(LENGTH_MEASURE(0.001),#9286,
'DISTANCE_ACCURACY_VALUE',
'Maximum model space distance between geometric entities at asserted c
onnectivities');
#9233=UNCERTAINTY_MEASURE_WITH_UNIT(LENGTH_MEASURE(0.001),#9286,
'DISTANCE_ACCURACY_VALUE',
'Maximum model space distance between geometric entities at asserted c
onnectivities');
#9234=UNCERTAINTY_MEASURE_WITH_UNIT(LENGTH_MEASURE(0.001),#9286,
'DISTANCE_ACCURACY_VALUE',
'Maximum model space distance between geometric entities at asserted c
onnectivities');
#9235=UNCERTAINTY_MEASURE_WITH_UNIT(LENGTH_MEASURE(0.001),#9286,
'DISTANCE_ACCURACY_VALUE',
'Maximum model space distance between geometric entities at asserted c
onnectivities');
#9236=UNCERTAINTY_MEASURE_WITH_UNIT(LENGTH_MEASURE(0.001),#9286,
'DISTANCE_ACCURACY_VALUE',
'Maximum model space distance between geometric entities at asserted c
onnectivities');
#9237=UNCERTAINTY_MEASURE_WITH_UNIT(LENGTH_MEASURE(0.001),#9286,
'DISTANCE_ACCURACY_VALUE',
'Maximum model space distance between geometric entities at asserted c
onnectivities');
#9238=UNCERTAINTY_MEASURE_WITH_UNIT(LENGTH_MEASURE(0.001),#9286,
'DISTANCE_ACCURACY_VALUE',
'Maximum model space distance between geometric entities at asserted c
onnectivities');
#9239=UNCERTAINTY_MEASURE_WITH_UNIT(LENGTH_MEASURE(0.001),#9286,
'DISTANCE_ACCURACY_VALUE',
'Maximum model space distance between geometric entities at asserted c
onnectivities');
#9240=UNCERTAINTY_MEASURE_WITH_UNIT(LENGTH_MEASURE(0.001),#9286,
'DISTANCE_ACCURACY_VALUE',
'Maximum model space distance between geometric entities at asserted c
onnectivities');
#9241=UNCERTAINTY_MEASURE_WITH_UNIT(LENGTH_MEASURE(0.001),#9286,
'DISTANCE_ACCURACY_VALUE',
'Maximum model space distance between geometric entities at asserted c
onnectivities');
#9242=UNCERTAINTY_MEASURE_WITH_UNIT(LENGTH_MEASURE(0.001),#9286,
'DISTANCE_ACCURACY_VALUE',
'Maximum model space distance between geometric entities at asserted c
onnectivities');
#9243=UNCERTAINTY_MEASURE_WITH_UNIT(LENGTH_MEASURE(0.001),#9286,
'DISTANCE_ACCURACY_VALUE',
'Maximum model space distance between geometric entities at asserted c
onnectivities');
#9244=UNCERTAINTY_MEASURE_WITH_UNIT(LENGTH_MEASURE(0.001),#9286,
'DISTANCE_ACCURACY_VALUE',
'Maximum model space distance between geometric entities at asserted c
onnectivities');
#9245=UNCERTAINTY_MEASURE_WITH_UNIT(LENGTH_MEASURE(0.001),#9286,
'DISTANCE_ACCURACY_VALUE',
'Maximum model space distance between geometric entities at asserted c
onnectivities');
#9246=UNCERTAINTY_MEASURE_WITH_UNIT(LENGTH_MEASURE(0.001),#9286,
'DISTANCE_ACCURACY_VALUE',
'Maximum model space distance between geometric entities at asserted c
onnectivities');
#9247=UNCERTAINTY_MEASURE_WITH_UNIT(LENGTH_MEASURE(0.001),#9286,
'DISTANCE_ACCURACY_VALUE',
'Maximum model space distance between geometric entities at asserted c
onnectivities');
#9248=UNCERTAINTY_MEASURE_WITH_UNIT(LENGTH_MEASURE(0.001),#9286,
'DISTANCE_ACCURACY_VALUE',
'Maximum model space distance between geometric entities at asserted c
onnectivities');
#9249=UNCERTAINTY_MEASURE_WITH_UNIT(LENGTH_MEASURE(0.001),#9286,
'DISTANCE_ACCURACY_VALUE',
'Maximum model space distance between geometric entities at asserted c
onnectivities');
#9250=UNCERTAINTY_MEASURE_WITH_UNIT(LENGTH_MEASURE(0.001),#9286,
'DISTANCE_ACCURACY_VALUE',
'Maximum model space distance between geometric entities at asserted c
onnectivities');
#9251=UNCERTAINTY_MEASURE_WITH_UNIT(LENGTH_MEASURE(0.001),#9286,
'DISTANCE_ACCURACY_VALUE',
'Maximum model space distance between geometric entities at asserted c
onnectivities');
#9252=UNCERTAINTY_MEASURE_WITH_UNIT(LENGTH_MEASURE(0.001),#9286,
'DISTANCE_ACCURACY_VALUE',
'Maximum model space distance between geometric entities at asserted c
onnectivities');
#9253=UNCERTAINTY_MEASURE_WITH_UNIT(LENGTH_MEASURE(0.001),#9286,
'DISTANCE_ACCURACY_VALUE',
'Maximum model space distance between geometric entities at asserted c
onnectivities');
#9254=UNCERTAINTY_MEASURE_WITH_UNIT(LENGTH_MEASURE(0.001),#9286,
'DISTANCE_ACCURACY_VALUE',
'Maximum model space distance between geometric entities at asserted c
onnectivities');
#9255=UNCERTAINTY_MEASURE_WITH_UNIT(LENGTH_MEASURE(0.001),#9286,
'DISTANCE_ACCURACY_VALUE',
'Maximum model space distance between geometric entities at asserted c
onnectivities');
#9256=(
GEOMETRIC_REPRESENTATION_CONTEXT(3)
GLOBAL_UNCERTAINTY_ASSIGNED_CONTEXT((#9226))
GLOBAL_UNIT_ASSIGNED_CONTEXT((#9286,#9288,#9289))
REPRESENTATION_CONTEXT('','3D')
);
#9257=(
GEOMETRIC_REPRESENTATION_CONTEXT(3)
GLOBAL_UNCERTAINTY_ASSIGNED_CONTEXT((#9227))
GLOBAL_UNIT_ASSIGNED_CONTEXT((#9286,#9288,#9289))
REPRESENTATION_CONTEXT('','3D')
);
#9258=(
GEOMETRIC_REPRESENTATION_CONTEXT(3)
GLOBAL_UNCERTAINTY_ASSIGNED_CONTEXT((#9228))
GLOBAL_UNIT_ASSIGNED_CONTEXT((#9286,#9288,#9289))
REPRESENTATION_CONTEXT('','3D')
);
#9259=(
GEOMETRIC_REPRESENTATION_CONTEXT(3)
GLOBAL_UNCERTAINTY_ASSIGNED_CONTEXT((#9229))
GLOBAL_UNIT_ASSIGNED_CONTEXT((#9286,#9288,#9289))
REPRESENTATION_CONTEXT('','3D')
);
#9260=(
GEOMETRIC_REPRESENTATION_CONTEXT(3)
GLOBAL_UNCERTAINTY_ASSIGNED_CONTEXT((#9230))
GLOBAL_UNIT_ASSIGNED_CONTEXT((#9286,#9288,#9289))
REPRESENTATION_CONTEXT('','3D')
);
#9261=(
GEOMETRIC_REPRESENTATION_CONTEXT(3)
GLOBAL_UNCERTAINTY_ASSIGNED_CONTEXT((#9231))
GLOBAL_UNIT_ASSIGNED_CONTEXT((#9286,#9288,#9289))
REPRESENTATION_CONTEXT('','3D')
);
#9262=(
GEOMETRIC_REPRESENTATION_CONTEXT(3)
GLOBAL_UNCERTAINTY_ASSIGNED_CONTEXT((#9232))
GLOBAL_UNIT_ASSIGNED_CONTEXT((#9286,#9288,#9289))
REPRESENTATION_CONTEXT('','3D')
);
#9263=(
GEOMETRIC_REPRESENTATION_CONTEXT(3)
GLOBAL_UNCERTAINTY_ASSIGNED_CONTEXT((#9233))
GLOBAL_UNIT_ASSIGNED_CONTEXT((#9286,#9288,#9289))
REPRESENTATION_CONTEXT('','3D')
);
#9264=(
GEOMETRIC_REPRESENTATION_CONTEXT(3)
GLOBAL_UNCERTAINTY_ASSIGNED_CONTEXT((#9234))
GLOBAL_UNIT_ASSIGNED_CONTEXT((#9286,#9288,#9289))
REPRESENTATION_CONTEXT('','3D')
);
#9265=(
GEOMETRIC_REPRESENTATION_CONTEXT(3)
GLOBAL_UNCERTAINTY_ASSIGNED_CONTEXT((#9235))
GLOBAL_UNIT_ASSIGNED_CONTEXT((#9286,#9288,#9289))
REPRESENTATION_CONTEXT('','3D')
);
#9266=(
GEOMETRIC_REPRESENTATION_CONTEXT(3)
GLOBAL_UNCERTAINTY_ASSIGNED_CONTEXT((#9236))
GLOBAL_UNIT_ASSIGNED_CONTEXT((#9286,#9288,#9289))
REPRESENTATION_CONTEXT('','3D')
);
#9267=(
GEOMETRIC_REPRESENTATION_CONTEXT(3)
GLOBAL_UNCERTAINTY_ASSIGNED_CONTEXT((#9237))
GLOBAL_UNIT_ASSIGNED_CONTEXT((#9286,#9288,#9289))
REPRESENTATION_CONTEXT('','3D')
);
#9268=(
GEOMETRIC_REPRESENTATION_CONTEXT(3)
GLOBAL_UNCERTAINTY_ASSIGNED_CONTEXT((#9238))
GLOBAL_UNIT_ASSIGNED_CONTEXT((#9286,#9288,#9289))
REPRESENTATION_CONTEXT('','3D')
);
#9269=(
GEOMETRIC_REPRESENTATION_CONTEXT(3)
GLOBAL_UNCERTAINTY_ASSIGNED_CONTEXT((#9239))
GLOBAL_UNIT_ASSIGNED_CONTEXT((#9286,#9288,#9289))
REPRESENTATION_CONTEXT('','3D')
);
#9270=(
GEOMETRIC_REPRESENTATION_CONTEXT(3)
GLOBAL_UNCERTAINTY_ASSIGNED_CONTEXT((#9240))
GLOBAL_UNIT_ASSIGNED_CONTEXT((#9286,#9288,#9289))
REPRESENTATION_CONTEXT('','3D')
);
#9271=(
GEOMETRIC_REPRESENTATION_CONTEXT(3)
GLOBAL_UNCERTAINTY_ASSIGNED_CONTEXT((#9241))
GLOBAL_UNIT_ASSIGNED_CONTEXT((#9286,#9288,#9289))
REPRESENTATION_CONTEXT('','3D')
);
#9272=(
GEOMETRIC_REPRESENTATION_CONTEXT(3)
GLOBAL_UNCERTAINTY_ASSIGNED_CONTEXT((#9242))
GLOBAL_UNIT_ASSIGNED_CONTEXT((#9286,#9288,#9289))
REPRESENTATION_CONTEXT('','3D')
);
#9273=(
GEOMETRIC_REPRESENTATION_CONTEXT(3)
GLOBAL_UNCERTAINTY_ASSIGNED_CONTEXT((#9243))
GLOBAL_UNIT_ASSIGNED_CONTEXT((#9286,#9288,#9289))
REPRESENTATION_CONTEXT('','3D')
);
#9274=(
GEOMETRIC_REPRESENTATION_CONTEXT(3)
GLOBAL_UNCERTAINTY_ASSIGNED_CONTEXT((#9244))
GLOBAL_UNIT_ASSIGNED_CONTEXT((#9286,#9288,#9289))
REPRESENTATION_CONTEXT('','3D')
);
#9275=(
GEOMETRIC_REPRESENTATION_CONTEXT(3)
GLOBAL_UNCERTAINTY_ASSIGNED_CONTEXT((#9245))
GLOBAL_UNIT_ASSIGNED_CONTEXT((#9286,#9288,#9289))
REPRESENTATION_CONTEXT('','3D')
);
#9276=(
GEOMETRIC_REPRESENTATION_CONTEXT(3)
GLOBAL_UNCERTAINTY_ASSIGNED_CONTEXT((#9246))
GLOBAL_UNIT_ASSIGNED_CONTEXT((#9286,#9288,#9289))
REPRESENTATION_CONTEXT('','3D')
);
#9277=(
GEOMETRIC_REPRESENTATION_CONTEXT(3)
GLOBAL_UNCERTAINTY_ASSIGNED_CONTEXT((#9247))
GLOBAL_UNIT_ASSIGNED_CONTEXT((#9286,#9288,#9289))
REPRESENTATION_CONTEXT('','3D')
);
#9278=(
GEOMETRIC_REPRESENTATION_CONTEXT(3)
GLOBAL_UNCERTAINTY_ASSIGNED_CONTEXT((#9248))
GLOBAL_UNIT_ASSIGNED_CONTEXT((#9286,#9288,#9289))
REPRESENTATION_CONTEXT('','3D')
);
#9279=(
GEOMETRIC_REPRESENTATION_CONTEXT(3)
GLOBAL_UNCERTAINTY_ASSIGNED_CONTEXT((#9249))
GLOBAL_UNIT_ASSIGNED_CONTEXT((#9286,#9288,#9289))
REPRESENTATION_CONTEXT('','3D')
);
#9280=(
GEOMETRIC_REPRESENTATION_CONTEXT(3)
GLOBAL_UNCERTAINTY_ASSIGNED_CONTEXT((#9250))
GLOBAL_UNIT_ASSIGNED_CONTEXT((#9286,#9288,#9289))
REPRESENTATION_CONTEXT('','3D')
);
#9281=(
GEOMETRIC_REPRESENTATION_CONTEXT(3)
GLOBAL_UNCERTAINTY_ASSIGNED_CONTEXT((#9251))
GLOBAL_UNIT_ASSIGNED_CONTEXT((#9286,#9288,#9289))
REPRESENTATION_CONTEXT('','3D')
);
#9282=(
GEOMETRIC_REPRESENTATION_CONTEXT(3)
GLOBAL_UNCERTAINTY_ASSIGNED_CONTEXT((#9252))
GLOBAL_UNIT_ASSIGNED_CONTEXT((#9286,#9288,#9289))
REPRESENTATION_CONTEXT('','3D')
);
#9283=(
GEOMETRIC_REPRESENTATION_CONTEXT(3)
GLOBAL_UNCERTAINTY_ASSIGNED_CONTEXT((#9253))
GLOBAL_UNIT_ASSIGNED_CONTEXT((#9286,#9288,#9289))
REPRESENTATION_CONTEXT('','3D')
);
#9284=(
GEOMETRIC_REPRESENTATION_CONTEXT(3)
GLOBAL_UNCERTAINTY_ASSIGNED_CONTEXT((#9254))
GLOBAL_UNIT_ASSIGNED_CONTEXT((#9286,#9288,#9289))
REPRESENTATION_CONTEXT('','3D')
);
#9285=(
GEOMETRIC_REPRESENTATION_CONTEXT(3)
GLOBAL_UNCERTAINTY_ASSIGNED_CONTEXT((#9255))
GLOBAL_UNIT_ASSIGNED_CONTEXT((#9286,#9288,#9289))
REPRESENTATION_CONTEXT('','3D')
);
#9286=(
LENGTH_UNIT()
NAMED_UNIT(*)
SI_UNIT(.CENTI.,.METRE.)
);
#9287=(
LENGTH_UNIT()
NAMED_UNIT(*)
SI_UNIT($,.METRE.)
);
#9288=(
NAMED_UNIT(*)
PLANE_ANGLE_UNIT()
SI_UNIT($,.RADIAN.)
);
#9289=(
NAMED_UNIT(*)
SI_UNIT($,.STERADIAN.)
SOLID_ANGLE_UNIT()
);
#9290=SHAPE_DEFINITION_REPRESENTATION(#9319,#9394);
#9291=SHAPE_DEFINITION_REPRESENTATION(#9320,#9395);
#9292=SHAPE_DEFINITION_REPRESENTATION(#9321,#9396);
#9293=SHAPE_DEFINITION_REPRESENTATION(#9322,#9397);
#9294=SHAPE_DEFINITION_REPRESENTATION(#9323,#9398);
#9295=SHAPE_DEFINITION_REPRESENTATION(#9324,#9399);
#9296=SHAPE_DEFINITION_REPRESENTATION(#9325,#9400);
#9297=SHAPE_DEFINITION_REPRESENTATION(#9326,#9401);
#9298=SHAPE_DEFINITION_REPRESENTATION(#9327,#9402);
#9299=SHAPE_DEFINITION_REPRESENTATION(#9328,#9403);
#9300=SHAPE_DEFINITION_REPRESENTATION(#9329,#9404);
#9301=SHAPE_DEFINITION_REPRESENTATION(#9330,#9405);
#9302=SHAPE_DEFINITION_REPRESENTATION(#9331,#9406);
#9303=SHAPE_DEFINITION_REPRESENTATION(#9332,#9407);
#9304=SHAPE_DEFINITION_REPRESENTATION(#9333,#9408);
#9305=SHAPE_DEFINITION_REPRESENTATION(#9334,#9409);
#9306=SHAPE_DEFINITION_REPRESENTATION(#9335,#9410);
#9307=SHAPE_DEFINITION_REPRESENTATION(#9336,#9411);
#9308=SHAPE_DEFINITION_REPRESENTATION(#9337,#9412);
#9309=SHAPE_DEFINITION_REPRESENTATION(#9338,#9413);
#9310=SHAPE_DEFINITION_REPRESENTATION(#9340,#9414);
#9311=SHAPE_DEFINITION_REPRESENTATION(#9341,#9415);
#9312=SHAPE_DEFINITION_REPRESENTATION(#9342,#9416);
#9313=SHAPE_DEFINITION_REPRESENTATION(#9343,#9417);
#9314=SHAPE_DEFINITION_REPRESENTATION(#9344,#9418);
#9315=SHAPE_DEFINITION_REPRESENTATION(#9345,#9419);
#9316=SHAPE_DEFINITION_REPRESENTATION(#9346,#9420);
#9317=SHAPE_DEFINITION_REPRESENTATION(#9347,#9421);
#9318=SHAPE_DEFINITION_REPRESENTATION(#9348,#9422);
#9319=PRODUCT_DEFINITION_SHAPE('',$,#9424);
#9320=PRODUCT_DEFINITION_SHAPE('',$,#9425);
#9321=PRODUCT_DEFINITION_SHAPE('',$,#9426);
#9322=PRODUCT_DEFINITION_SHAPE('',$,#9427);
#9323=PRODUCT_DEFINITION_SHAPE('',$,#9428);
#9324=PRODUCT_DEFINITION_SHAPE('',$,#9429);
#9325=PRODUCT_DEFINITION_SHAPE('',$,#9430);
#9326=PRODUCT_DEFINITION_SHAPE('',$,#9431);
#9327=PRODUCT_DEFINITION_SHAPE('',$,#9432);
#9328=PRODUCT_DEFINITION_SHAPE('',$,#9433);
#9329=PRODUCT_DEFINITION_SHAPE('',$,#9434);
#9330=PRODUCT_DEFINITION_SHAPE('',$,#9435);
#9331=PRODUCT_DEFINITION_SHAPE('',$,#9436);
#9332=PRODUCT_DEFINITION_SHAPE('',$,#9437);
#9333=PRODUCT_DEFINITION_SHAPE('',$,#9438);
#9334=PRODUCT_DEFINITION_SHAPE('',$,#9439);
#9335=PRODUCT_DEFINITION_SHAPE('',$,#9440);
#9336=PRODUCT_DEFINITION_SHAPE('',$,#9441);
#9337=PRODUCT_DEFINITION_SHAPE('',$,#9442);
#9338=PRODUCT_DEFINITION_SHAPE('',$,#9443);
#9339=PRODUCT_DEFINITION_SHAPE($,$,#156);
#9340=PRODUCT_DEFINITION_SHAPE('',$,#9444);
#9341=PRODUCT_DEFINITION_SHAPE('',$,#9445);
#9342=PRODUCT_DEFINITION_SHAPE('',$,#9446);
#9343=PRODUCT_DEFINITION_SHAPE('',$,#9447);
#9344=PRODUCT_DEFINITION_SHAPE('',$,#9448);
#9345=PRODUCT_DEFINITION_SHAPE('',$,#9449);
#9346=PRODUCT_DEFINITION_SHAPE('',$,#9450);
#9347=PRODUCT_DEFINITION_SHAPE('',$,#9451);
#9348=PRODUCT_DEFINITION_SHAPE('',$,#9452);
#9349=PRODUCT_DEFINITION_SHAPE($,$,#157);
#9350=PRODUCT_DEFINITION_SHAPE($,$,#158);
#9351=PRODUCT_DEFINITION_SHAPE($,$,#159);
#9352=PRODUCT_DEFINITION_SHAPE($,$,#160);
#9353=PRODUCT_DEFINITION_SHAPE($,$,#161);
#9354=PRODUCT_DEFINITION_SHAPE($,$,#162);
#9355=PRODUCT_DEFINITION_SHAPE($,$,#163);
#9356=PRODUCT_DEFINITION_SHAPE($,$,#164);
#9357=PRODUCT_DEFINITION_SHAPE($,$,#165);
#9358=PRODUCT_DEFINITION_SHAPE($,$,#166);
#9359=PRODUCT_DEFINITION_SHAPE($,$,#167);
#9360=PRODUCT_DEFINITION_SHAPE($,$,#168);
#9361=PRODUCT_DEFINITION_SHAPE($,$,#169);
#9362=PRODUCT_DEFINITION_SHAPE($,$,#170);
#9363=PRODUCT_DEFINITION_SHAPE($,$,#171);
#9364=PRODUCT_DEFINITION_SHAPE($,$,#172);
#9365=PRODUCT_DEFINITION_SHAPE($,$,#173);
#9366=PRODUCT_DEFINITION_SHAPE($,$,#174);
#9367=PRODUCT_DEFINITION_SHAPE($,$,#175);
#9368=PRODUCT_DEFINITION_SHAPE($,$,#176);
#9369=PRODUCT_DEFINITION_SHAPE($,$,#177);
#9370=PRODUCT_DEFINITION_SHAPE($,$,#178);
#9371=PRODUCT_DEFINITION_SHAPE($,$,#179);
#9372=PRODUCT_DEFINITION_SHAPE($,$,#180);
#9373=PRODUCT_DEFINITION_SHAPE($,$,#181);
#9374=PRODUCT_DEFINITION_SHAPE($,$,#182);
#9375=PRODUCT_DEFINITION_SHAPE($,$,#183);
#9376=PRODUCT_DEFINITION_SHAPE($,$,#184);
#9377=PRODUCT_DEFINITION_SHAPE($,$,#185);
#9378=PRODUCT_DEFINITION_SHAPE($,$,#186);
#9379=PRODUCT_DEFINITION_SHAPE($,$,#187);
#9380=PRODUCT_DEFINITION_SHAPE($,$,#188);
#9381=PRODUCT_DEFINITION_SHAPE($,$,#189);
#9382=PRODUCT_DEFINITION_SHAPE($,$,#190);
#9383=PRODUCT_DEFINITION_SHAPE($,$,#191);
#9384=PRODUCT_DEFINITION_SHAPE($,$,#192);
#9385=PRODUCT_DEFINITION_SHAPE($,$,#193);
#9386=PRODUCT_DEFINITION_SHAPE($,$,#194);
#9387=PRODUCT_DEFINITION_SHAPE($,$,#195);
#9388=PRODUCT_DEFINITION_SHAPE($,$,#196);
#9389=PRODUCT_DEFINITION_SHAPE($,$,#197);
#9390=PRODUCT_DEFINITION_SHAPE($,$,#198);
#9391=PRODUCT_DEFINITION_SHAPE($,$,#199);
#9392=PRODUCT_DEFINITION_SHAPE($,$,#200);
#9393=PRODUCT_DEFINITION_SHAPE($,$,#201);
#9394=SHAPE_REPRESENTATION('',(#5461,#6025,#6026,#6027,#6028),#9256);
#9395=SHAPE_REPRESENTATION('',(#5462,#5984,#5985,#5986,#5987,#5988,#5989,
#5990,#5991,#5992,#5993,#5994,#5995,#5996,#5997,#5998,#5999,#6000,#6001,
#6002,#6003,#6004,#6005,#6006,#6007),#9257);
#9396=SHAPE_REPRESENTATION('',(#5463),#9258);
#9397=SHAPE_REPRESENTATION('',(#5511),#9259);
#9398=SHAPE_REPRESENTATION('',(#5546),#9260);
#9399=SHAPE_REPRESENTATION('',(#5557),#9261);
#9400=SHAPE_REPRESENTATION('',(#5581),#9262);
#9401=SHAPE_REPRESENTATION('',(#5672),#9263);
#9402=SHAPE_REPRESENTATION('',(#5685),#9264);
#9403=SHAPE_REPRESENTATION('',(#5702),#9265);
#9404=SHAPE_REPRESENTATION('',(#5718),#9266);
#9405=SHAPE_REPRESENTATION('',(#5728),#9267);
#9406=SHAPE_REPRESENTATION('',(#5736),#9268);
#9407=SHAPE_REPRESENTATION('',(#5754),#9269);
#9408=SHAPE_REPRESENTATION('',(#5778,#6008,#6009,#6010,#6011,#6012,#6013,
#6014,#6015),#9270);
#9409=SHAPE_REPRESENTATION('',(#5779),#9271);
#9410=SHAPE_REPRESENTATION('',(#5822),#9272);
#9411=SHAPE_REPRESENTATION('',(#5832),#9273);
#9412=SHAPE_REPRESENTATION('',(#5856,#5874),#9274);
#9413=SHAPE_REPRESENTATION('',(#5857),#9275);
#9414=SHAPE_REPRESENTATION('',(#5875,#6016,#6017,#6018,#6019,#6020,#6021,
#6022,#6023,#6024),#9276);
#9415=SHAPE_REPRESENTATION('',(#5876),#9277);
#9416=SHAPE_REPRESENTATION('',(#5901),#9278);
#9417=SHAPE_REPRESENTATION('',(#5918),#9279);
#9418=SHAPE_REPRESENTATION('',(#5934),#9280);
#9419=SHAPE_REPRESENTATION('',(#5940),#9281);
#9420=SHAPE_REPRESENTATION('',(#5955),#9282);
#9421=SHAPE_REPRESENTATION('',(#5964),#9283);
#9422=SHAPE_REPRESENTATION('',(#5973),#9284);
#9423=PRODUCT_DEFINITION_CONTEXT('part definition',#9512,'design');
#9424=PRODUCT_DEFINITION('PAT-069',
'PAT-069',#9453,#9423);
#9425=PRODUCT_DEFINITION('Base guide and handle stop',
'Base guide and handle stop',#9454,#9423);
#9426=PRODUCT_DEFINITION('Twenty-five millimetre clamp base',
'Twenty-five millimetre clamp base',#9455,#9423);
#9427=PRODUCT_DEFINITION('Bolt-clearance mounting stand',
'Bolt-clearance mounting stand',#9456,#9423);
#9428=PRODUCT_DEFINITION('Flat Washer - M5','Flat Washer - M5',#9457,#9423);
#9429=PRODUCT_DEFINITION('M5x14 Cap Screw','M5x14 Cap Screw',#9458,#9423);
#9430=PRODUCT_DEFINITION('Located grid plate','Located grid plate',#9459,
#9423);
#9431=PRODUCT_DEFINITION('Bolted edge stop','Bolted edge stop',#9460,#9423);
#9432=PRODUCT_DEFINITION('Hex Bolt - M6 x 30 mm',
'Hex Bolt - M6 x 30 mm',#9461,#9423);
#9433=PRODUCT_DEFINITION('Hex Nut - M6','Hex Nut - M6',#9462,#9423);
#9434=PRODUCT_DEFINITION('Rest button','Rest button',#9463,#9423);
#9435=PRODUCT_DEFINITION('Dowel Pin - 6x30','Dowel Pin - 6x30',#9464,#9423);
#9436=PRODUCT_DEFINITION('Relieved diamond locating pin',
'Relieved diamond locating pin',#9465,#9423);
#9437=PRODUCT_DEFINITION('M8x25 Bolt','M8x25 Bolt',#9466,#9423);
#9438=PRODUCT_DEFINITION('Operating crank','Operating crank',#9467,#9423);
#9439=PRODUCT_DEFINITION('Operating lever','Operating lever',#9468,#9423);
#9440=PRODUCT_DEFINITION('Handle','Handle',#9469,#9423);
#9441=PRODUCT_DEFINITION('M5x14 Cap Screw (1)','M5x14 Cap Screw (1)',#9470,
#9423);
#9442=PRODUCT_DEFINITION('Toggle connecting link',
'Toggle connecting link',#9471,#9423);
#9443=PRODUCT_DEFINITION('Thirty-five millimetre toggle link',
'Thirty-five millimetre toggle link',#9472,#9423);
#9444=PRODUCT_DEFINITION('Plunger and M8 spindle',
'Plunger and M8 spindle',#9473,#9423);
#9445=PRODUCT_DEFINITION('Forked pressure plunger',
'Forked pressure plunger',#9474,#9423);
#9446=PRODUCT_DEFINITION('Hex Bolt - M8x40','Hex Bolt - M8x40',#9475,#9423);
#9447=PRODUCT_DEFINITION('Hex Nut - M8','Hex Nut - M8',#9476,#9423);
#9448=PRODUCT_DEFINITION('Elastomer pressure pad installed',
'Elastomer pressure pad installed',#9477,#9423);
#9449=PRODUCT_DEFINITION('Clevis Pin - 6x30','Clevis Pin - 6x30',#9478,
#9423);
#9450=PRODUCT_DEFINITION('Flat Washer - M6','Flat Washer - M6',#9479,#9423);
#9451=PRODUCT_DEFINITION('Pivot retention spacer',
'Pivot retention spacer',#9480,#9423);
#9452=PRODUCT_DEFINITION('Split Pin - 1.6x16','Split Pin - 1.6x16',#9481,
#9423);
#9453=PRODUCT_DEFINITION_FORMATION('',$,#9514);
#9454=PRODUCT_DEFINITION_FORMATION('',$,#9515);
#9455=PRODUCT_DEFINITION_FORMATION('',$,#9516);
#9456=PRODUCT_DEFINITION_FORMATION('',$,#9517);
#9457=PRODUCT_DEFINITION_FORMATION('',$,#9518);
#9458=PRODUCT_DEFINITION_FORMATION('',$,#9519);
#9459=PRODUCT_DEFINITION_FORMATION('',$,#9520);
#9460=PRODUCT_DEFINITION_FORMATION('',$,#9521);
#9461=PRODUCT_DEFINITION_FORMATION('',$,#9522);
#9462=PRODUCT_DEFINITION_FORMATION('',$,#9523);
#9463=PRODUCT_DEFINITION_FORMATION('',$,#9524);
#9464=PRODUCT_DEFINITION_FORMATION('',$,#9525);
#9465=PRODUCT_DEFINITION_FORMATION('',$,#9526);
#9466=PRODUCT_DEFINITION_FORMATION('',$,#9527);
#9467=PRODUCT_DEFINITION_FORMATION('',$,#9528);
#9468=PRODUCT_DEFINITION_FORMATION('',$,#9529);
#9469=PRODUCT_DEFINITION_FORMATION('',$,#9530);
#9470=PRODUCT_DEFINITION_FORMATION('',$,#9531);
#9471=PRODUCT_DEFINITION_FORMATION('',$,#9532);
#9472=PRODUCT_DEFINITION_FORMATION('',$,#9533);
#9473=PRODUCT_DEFINITION_FORMATION('',$,#9534);
#9474=PRODUCT_DEFINITION_FORMATION('',$,#9535);
#9475=PRODUCT_DEFINITION_FORMATION('',$,#9536);
#9476=PRODUCT_DEFINITION_FORMATION('',$,#9537);
#9477=PRODUCT_DEFINITION_FORMATION('',$,#9538);
#9478=PRODUCT_DEFINITION_FORMATION('',$,#9539);
#9479=PRODUCT_DEFINITION_FORMATION('',$,#9540);
#9480=PRODUCT_DEFINITION_FORMATION('',$,#9541);
#9481=PRODUCT_DEFINITION_FORMATION('',$,#9542);
#9482=PRODUCT_RELATED_PRODUCT_CATEGORY('PAT-069','PAT-069',(#9514));
#9483=PRODUCT_RELATED_PRODUCT_CATEGORY('Base guide and handle stop',
'Base guide and handle stop',(#9515));
#9484=PRODUCT_RELATED_PRODUCT_CATEGORY(
'Twenty-five millimetre clamp base','Twenty-five millimetre clamp base',
(#9516));
#9485=PRODUCT_RELATED_PRODUCT_CATEGORY('Bolt-clearance mounting stand',
'Bolt-clearance mounting stand',(#9517));
#9486=PRODUCT_RELATED_PRODUCT_CATEGORY('Flat Washer - M5',
'Flat Washer - M5',(#9518));
#9487=PRODUCT_RELATED_PRODUCT_CATEGORY('M5x14 Cap Screw',
'M5x14 Cap Screw',(#9519));
#9488=PRODUCT_RELATED_PRODUCT_CATEGORY('Located grid plate',
'Located grid plate',(#9520));
#9489=PRODUCT_RELATED_PRODUCT_CATEGORY('Bolted edge stop',
'Bolted edge stop',(#9521));
#9490=PRODUCT_RELATED_PRODUCT_CATEGORY('Hex Bolt - M6 x 30 mm',
'Hex Bolt - M6 x 30 mm',(#9522));
#9491=PRODUCT_RELATED_PRODUCT_CATEGORY('Hex Nut - M6','Hex Nut - M6',(#9523));
#9492=PRODUCT_RELATED_PRODUCT_CATEGORY('Rest button','Rest button',(#9524));
#9493=PRODUCT_RELATED_PRODUCT_CATEGORY('Dowel Pin - 6x30',
'Dowel Pin - 6x30',(#9525));
#9494=PRODUCT_RELATED_PRODUCT_CATEGORY('Relieved diamond locating pin',
'Relieved diamond locating pin',(#9526));
#9495=PRODUCT_RELATED_PRODUCT_CATEGORY('M8x25 Bolt','M8x25 Bolt',(#9527));
#9496=PRODUCT_RELATED_PRODUCT_CATEGORY('Operating crank',
'Operating crank',(#9528));
#9497=PRODUCT_RELATED_PRODUCT_CATEGORY('Operating lever',
'Operating lever',(#9529));
#9498=PRODUCT_RELATED_PRODUCT_CATEGORY('Handle','Handle',(#9530));
#9499=PRODUCT_RELATED_PRODUCT_CATEGORY('M5x14 Cap Screw (1)',
'M5x14 Cap Screw (1)',(#9531));
#9500=PRODUCT_RELATED_PRODUCT_CATEGORY('Toggle connecting link',
'Toggle connecting link',(#9532));
#9501=PRODUCT_RELATED_PRODUCT_CATEGORY(
'Thirty-five millimetre toggle link',
'Thirty-five millimetre toggle link',(#9533));
#9502=PRODUCT_RELATED_PRODUCT_CATEGORY('Plunger and M8 spindle',
'Plunger and M8 spindle',(#9534));
#9503=PRODUCT_RELATED_PRODUCT_CATEGORY('Forked pressure plunger',
'Forked pressure plunger',(#9535));
#9504=PRODUCT_RELATED_PRODUCT_CATEGORY('Hex Bolt - M8x40',
'Hex Bolt - M8x40',(#9536));
#9505=PRODUCT_RELATED_PRODUCT_CATEGORY('Hex Nut - M8','Hex Nut - M8',(#9537));
#9506=PRODUCT_RELATED_PRODUCT_CATEGORY(
'Elastomer pressure pad installed','Elastomer pressure pad installed',(#9538));
#9507=PRODUCT_RELATED_PRODUCT_CATEGORY('Clevis Pin - 6x30',
'Clevis Pin - 6x30',(#9539));
#9508=PRODUCT_RELATED_PRODUCT_CATEGORY('Flat Washer - M6',
'Flat Washer - M6',(#9540));
#9509=PRODUCT_RELATED_PRODUCT_CATEGORY('Pivot retention spacer',
'Pivot retention spacer',(#9541));
#9510=PRODUCT_RELATED_PRODUCT_CATEGORY('Split Pin - 1.6x16',
'Split Pin - 1.6x16',(#9542));
#9511=APPLICATION_PROTOCOL_DEFINITION('international standard',
'automotive_design',2009,#9512);
#9512=APPLICATION_CONTEXT(
'Core Data for Automotive Mechanical Design Process');
#9513=PRODUCT_CONTEXT('part definition',#9512,'mechanical');
#9514=PRODUCT('PAT-069','PAT-069',
'PAT-069',(#9513));
#9515=PRODUCT('Base guide and handle stop','Base guide and handle stop',
'Base guide and handle stop',(#9513));
#9516=PRODUCT('Twenty-five millimetre clamp base',
'Twenty-five millimetre clamp base','Twenty-five millimetre clamp base',
(#9513));
#9517=PRODUCT('Bolt-clearance mounting stand',
'Bolt-clearance mounting stand','Bolt-clearance mounting stand',(#9513));
#9518=PRODUCT('Flat Washer - M5','Flat Washer - M5','Flat Washer - M5',
(#9513));
#9519=PRODUCT('M5x14 Cap Screw','M5x14 Cap Screw','M5x14 Cap Screw',(#9513));
#9520=PRODUCT('Located grid plate','Located grid plate',
'Located grid plate',(#9513));
#9521=PRODUCT('Bolted edge stop','Bolted edge stop','Bolted edge stop',
(#9513));
#9522=PRODUCT('Hex Bolt - M6 x 30 mm','Hex Bolt - M6 x 30 mm',
'Hex Bolt - M6 x 30 mm',(#9513));
#9523=PRODUCT('Hex Nut - M6','Hex Nut - M6','Hex Nut - M6',(#9513));
#9524=PRODUCT('Rest button','Rest button','Rest button',(#9513));
#9525=PRODUCT('Dowel Pin - 6x30','Dowel Pin - 6x30','Dowel Pin - 6x30',
(#9513));
#9526=PRODUCT('Relieved diamond locating pin',
'Relieved diamond locating pin','Relieved diamond locating pin',(#9513));
#9527=PRODUCT('M8x25 Bolt','M8x25 Bolt','M8x25 Bolt',(#9513));
#9528=PRODUCT('Operating crank','Operating crank','Operating crank',(#9513));
#9529=PRODUCT('Operating lever','Operating lever','Operating lever',(#9513));
#9530=PRODUCT('Handle','Handle','Handle',(#9513));
#9531=PRODUCT('M5x14 Cap Screw (1)','M5x14 Cap Screw (1)',
'M5x14 Cap Screw (1)',(#9513));
#9532=PRODUCT('Toggle connecting link','Toggle connecting link',
'Toggle connecting link',(#9513));
#9533=PRODUCT('Thirty-five millimetre toggle link',
'Thirty-five millimetre toggle link',
'Thirty-five millimetre toggle link',(#9513));
#9534=PRODUCT('Plunger and M8 spindle','Plunger and M8 spindle',
'Plunger and M8 spindle',(#9513));
#9535=PRODUCT('Forked pressure plunger','Forked pressure plunger',
'Forked pressure plunger',(#9513));
#9536=PRODUCT('Hex Bolt - M8x40','Hex Bolt - M8x40','Hex Bolt - M8x40',
(#9513));
#9537=PRODUCT('Hex Nut - M8','Hex Nut - M8','Hex Nut - M8',(#9513));
#9538=PRODUCT('Elastomer pressure pad installed',
'Elastomer pressure pad installed','Elastomer pressure pad installed',(#9513));
#9539=PRODUCT('Clevis Pin - 6x30','Clevis Pin - 6x30',
'Clevis Pin - 6x30',(#9513));
#9540=PRODUCT('Flat Washer - M6','Flat Washer - M6','Flat Washer - M6',
(#9513));
#9541=PRODUCT('Pivot retention spacer','Pivot retention spacer',
'Pivot retention spacer',(#9513));
#9542=PRODUCT('Split Pin - 1.6x16','Split Pin - 1.6x16',
'Split Pin - 1.6x16',(#9513));
#9543=PRESENTATION_STYLE_ASSIGNMENT((#9549));
#9544=PRESENTATION_STYLE_ASSIGNMENT((#9550));
#9545=PRESENTATION_STYLE_ASSIGNMENT((#9551));
#9546=PRESENTATION_STYLE_ASSIGNMENT((#9552));
#9547=PRESENTATION_STYLE_ASSIGNMENT((#9553));
#9548=PRESENTATION_STYLE_ASSIGNMENT((#9554));
#9549=SURFACE_STYLE_USAGE(.BOTH.,#9555);
#9550=SURFACE_STYLE_USAGE(.BOTH.,#9556);
#9551=SURFACE_STYLE_USAGE(.BOTH.,#9557);
#9552=SURFACE_STYLE_USAGE(.BOTH.,#9558);
#9553=SURFACE_STYLE_USAGE(.BOTH.,#9559);
#9554=SURFACE_STYLE_USAGE(.BOTH.,#9560);
#9555=SURFACE_SIDE_STYLE('',(#9561));
#9556=SURFACE_SIDE_STYLE('',(#9562));
#9557=SURFACE_SIDE_STYLE('',(#9563));
#9558=SURFACE_SIDE_STYLE('',(#9564));
#9559=SURFACE_SIDE_STYLE('',(#9565));
#9560=SURFACE_SIDE_STYLE('',(#9566));
#9561=SURFACE_STYLE_FILL_AREA(#9567);
#9562=SURFACE_STYLE_FILL_AREA(#9568);
#9563=SURFACE_STYLE_FILL_AREA(#9569);
#9564=SURFACE_STYLE_FILL_AREA(#9570);
#9565=SURFACE_STYLE_FILL_AREA(#9571);
#9566=SURFACE_STYLE_FILL_AREA(#9572);
#9567=FILL_AREA_STYLE('Steel - Satin',(#9573));
#9568=FILL_AREA_STYLE('CAD Library Painted - Deep blue',(#9574));
#9569=FILL_AREA_STYLE('CAD Library Painted - Graphite',(#9575));
#9570=FILL_AREA_STYLE('CAD Library Painted - Steel gray',(#9576));
#9571=FILL_AREA_STYLE('CAD Library Painted - Engineering blue',(#9577));
#9572=FILL_AREA_STYLE('CAD Library Painted - Light blue',(#9578));
#9573=FILL_AREA_STYLE_COLOUR('Steel - Satin',#9579);
#9574=FILL_AREA_STYLE_COLOUR('CAD Library Painted - Deep blue',#9580);
#9575=FILL_AREA_STYLE_COLOUR('CAD Library Painted - Graphite',#9581);
#9576=FILL_AREA_STYLE_COLOUR('CAD Library Painted - Steel gray',#9582);
#9577=FILL_AREA_STYLE_COLOUR('CAD Library Painted - Engineering blue',#9583);
#9578=FILL_AREA_STYLE_COLOUR('CAD Library Painted - Light blue',#9584);
#9579=COLOUR_RGB('Steel - Satin',0.627450980392157,0.627450980392157,0.627450980392157);
#9580=COLOUR_RGB('CAD Library Painted - Deep blue',0.0784313725490196,0.203921568627451,
0.349019607843137);
#9581=COLOUR_RGB('CAD Library Painted - Graphite',0.0980392156862745,0.109803921568627,
0.125490196078431);
#9582=COLOUR_RGB('CAD Library Painted - Steel gray',0.592156862745098,0.631372549019608,
0.67843137254902);
#9583=COLOUR_RGB('CAD Library Painted - Engineering blue',0.12156862745098,
0.356862745098039,0.6);
#9584=COLOUR_RGB('CAD Library Painted - Light blue',0.286274509803922,0.552941176470588,
0.780392156862745);
#9585=COLOUR_RGB('Dark Blue',0.08,0.2,0.34);
#9586=FILL_AREA_STYLE_COLOUR('',#9585);
#9587=FILL_AREA_STYLE('',(#9586));
#9588=SURFACE_STYLE_FILL_AREA(#9587);
#9589=SURFACE_SIDE_STYLE('',(#9588));
#9590=SURFACE_STYLE_USAGE(.BOTH.,#9589);
#9591=PRESENTATION_STYLE_ASSIGNMENT((#9590));
#9592=COLOUR_RGB('Light Blue',0.38,0.62,0.78);
#9593=FILL_AREA_STYLE_COLOUR('',#9592);
#9594=FILL_AREA_STYLE('',(#9593));
#9595=SURFACE_STYLE_FILL_AREA(#9594);
#9596=SURFACE_SIDE_STYLE('',(#9595));
#9597=SURFACE_STYLE_USAGE(.BOTH.,#9596);
#9598=PRESENTATION_STYLE_ASSIGNMENT((#9597));
#9599=COLOUR_RGB('Sky Blue',0.24,0.69,0.87);
#9600=FILL_AREA_STYLE_COLOUR('',#9599);
#9601=FILL_AREA_STYLE('',(#9600));
#9602=SURFACE_STYLE_FILL_AREA(#9601);
#9603=SURFACE_SIDE_STYLE('',(#9602));
#9604=SURFACE_STYLE_USAGE(.BOTH.,#9603);
#9605=PRESENTATION_STYLE_ASSIGNMENT((#9604));
#9606=COLOUR_RGB('Grey',0.48,0.52,0.57);
#9607=FILL_AREA_STYLE_COLOUR('',#9606);
#9608=FILL_AREA_STYLE('',(#9607));
#9609=SURFACE_STYLE_FILL_AREA(#9608);
#9610=SURFACE_SIDE_STYLE('',(#9609));
#9611=SURFACE_STYLE_USAGE(.BOTH.,#9610);
#9612=PRESENTATION_STYLE_ASSIGNMENT((#9611));
#9613=COLOUR_RGB('Black',0.12,0.14,0.17);
#9614=FILL_AREA_STYLE_COLOUR('',#9613);
#9615=FILL_AREA_STYLE('',(#9614));
#9616=SURFACE_STYLE_FILL_AREA(#9615);
#9617=SURFACE_SIDE_STYLE('',(#9616));
#9618=SURFACE_STYLE_USAGE(.BOTH.,#9617);
#9619=PRESENTATION_STYLE_ASSIGNMENT((#9618));
#9620=COLOUR_RGB('Off White',0.89,0.88,0.83);
#9621=FILL_AREA_STYLE_COLOUR('',#9620);
#9622=FILL_AREA_STYLE('',(#9621));
#9623=SURFACE_STYLE_FILL_AREA(#9622);
#9624=SURFACE_SIDE_STYLE('',(#9623));
#9625=SURFACE_STYLE_USAGE(.BOTH.,#9624);
#9626=PRESENTATION_STYLE_ASSIGNMENT((#9625));
ENDSEC;
END-ISO-10303-21;
